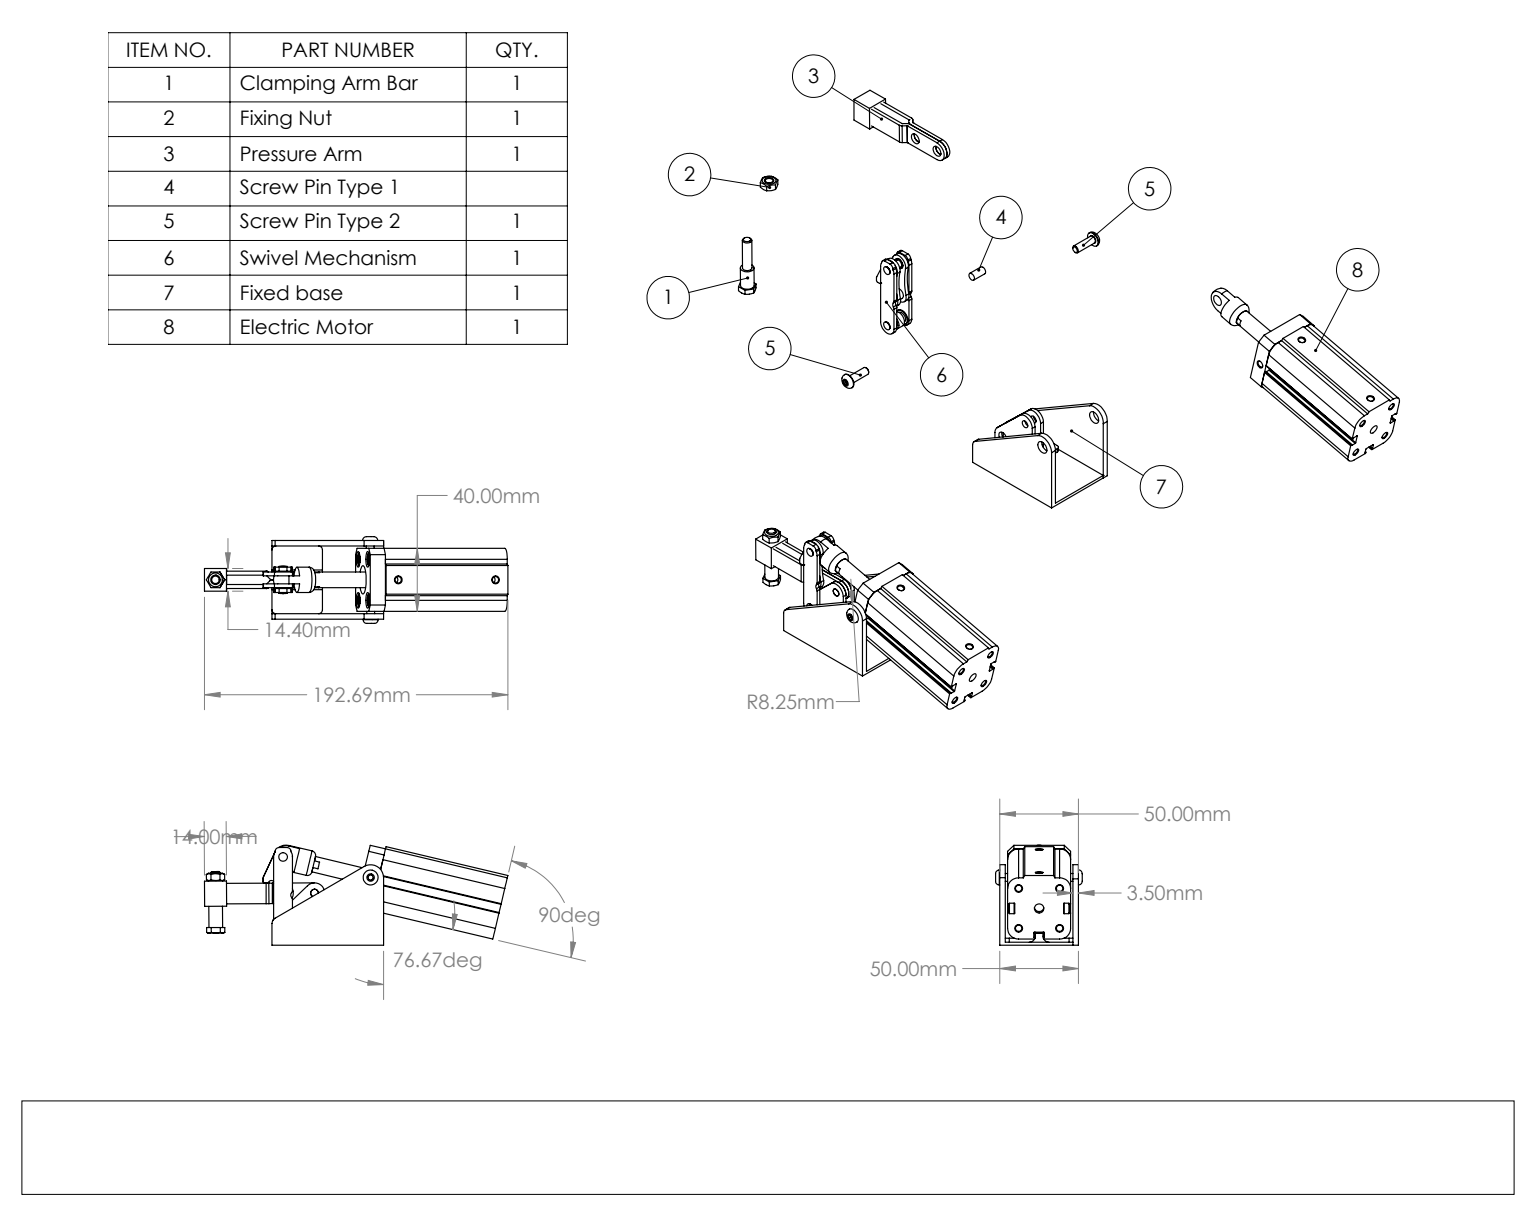
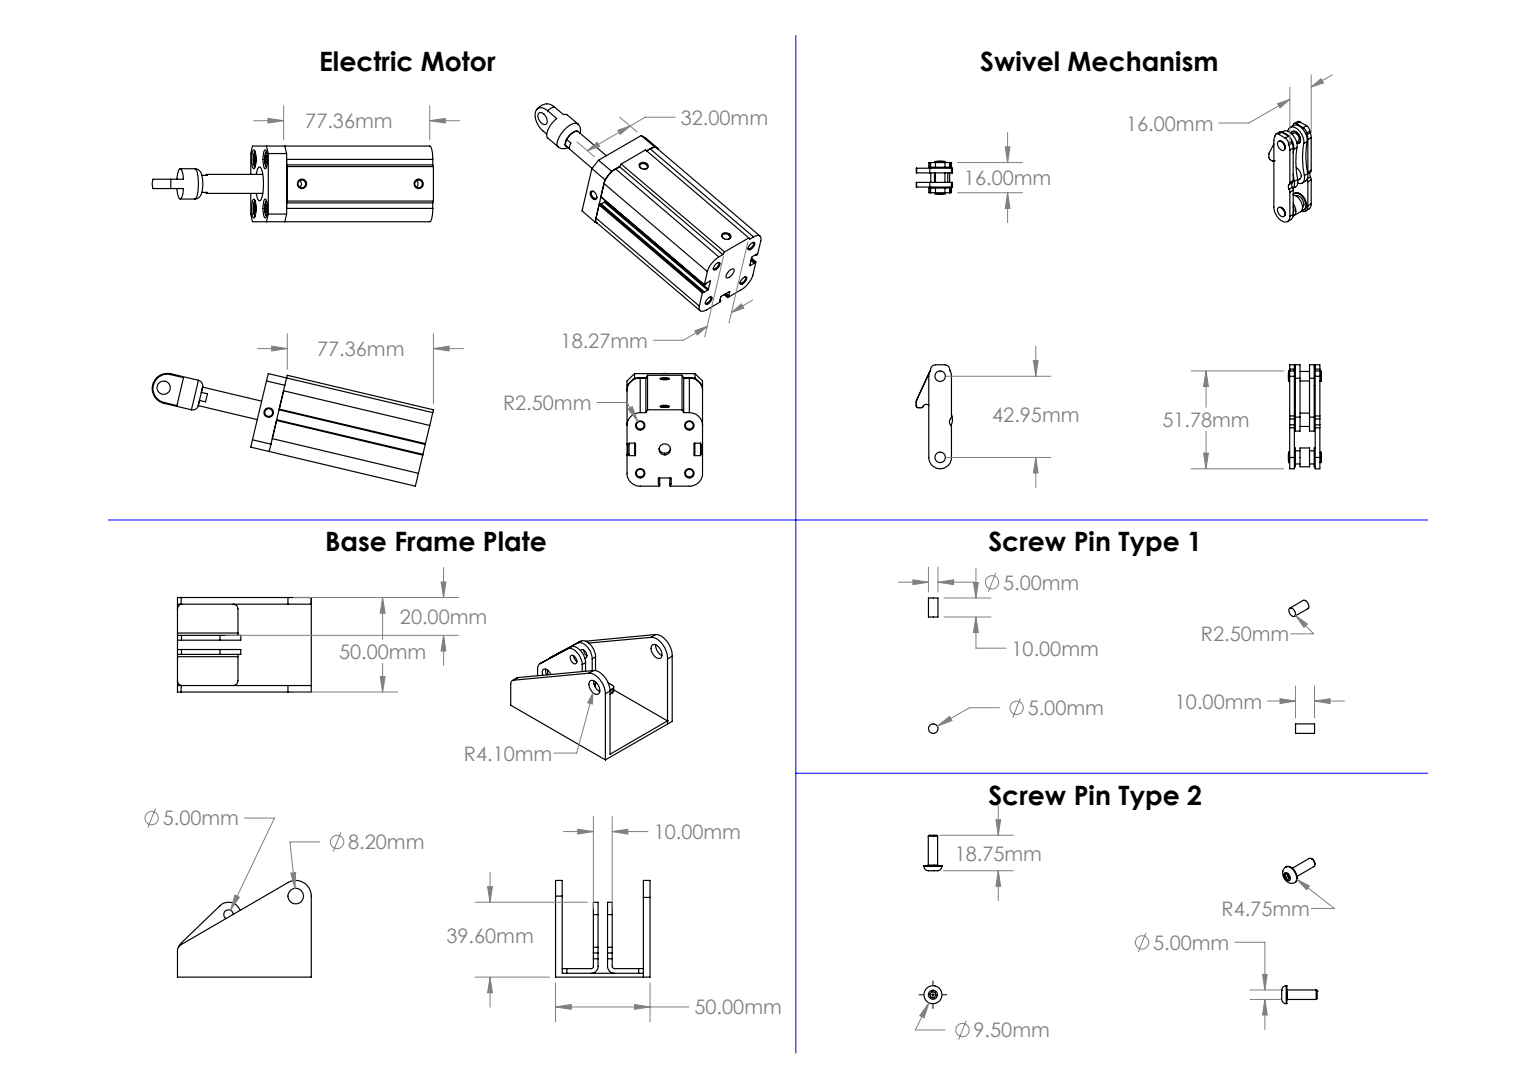
ISO-10303-21;
HEADER;
FILE_DESCRIPTION (('STEP AP203'),
    '1' );
FILE_NAME ('BR-Y-121',
    '2026-10-31T14:11:27',
    ( '' ),
    ( '' ),
    'SwSTEP 2.0',
    'SolidWorks 2024',
    '' );
FILE_SCHEMA (( 'AUTOMOTIVE_DESIGN' ));
ENDSEC;

DATA;
#1 = APPROVAL_PERSON_ORGANIZATION ( #6203, #14233, #2628 ) ;
#2 = DIRECTION ( 'NONE',  ( -0.9730401042858035643, 0.2306359803922028717, 5.958148513035547083E-17 ) ) ;
#3 = AXIS2_PLACEMENT_3D ( 'NONE', #15505, #7827, #17532 ) ;
#4 = DIRECTION ( 'NONE',  ( 1.000000000000000000, 0.000000000000000000, 0.000000000000000000 ) ) ;
#5 = CIRCLE ( 'NONE', #20894, 5.000000000000000000 ) ;
#6 = ORIENTED_EDGE ( 'NONE', *, *, #3696, .T. ) ;
#7 = PERSON ( 'NAUO-PER9', 'UNSPECIFIED', 'UNSPECIFIED', ('UNSPECIFIED'), ('UNSPECIFIED'), ('UNSPECIFIED') ) ;
#8 = CARTESIAN_POINT ( 'NONE',  ( -14.54830929633810044, -2.787889851644860251, 8.000000000004460432 ) ) ;
#9 = PERSON_AND_ORGANIZATION ( #11966, #8758 ) ;
#10 = FACE_OUTER_BOUND ( 'NONE', #10461, .T. ) ;
#11 = CARTESIAN_POINT ( 'NONE',  ( 34.15720538308221421, 9.344634530308759679, 27.44000000000022865 ) ) ;
#12 = CARTESIAN_POINT ( 'NONE',  ( 35.59419854219520118, 9.774809681453518806, 20.00000000000000000 ) ) ;
#13 = LOCAL_TIME ( 14, 11, 27.00000000000000000, #9898 ) ;
#14 = DIRECTION ( 'NONE',  ( -0.2306359803922088947, -0.9730401042858021210, 5.139921410301650007E-15 ) ) ;
#15 = CARTESIAN_POINT ( 'NONE',  ( -20.00000000000000000, -20.00000000000000000, 5.000000000004559908 ) ) ;
#16 = APPROVAL_PERSON_ORGANIZATION ( #20462, #778, #17266 ) ;
#17 = ORIENTED_EDGE ( 'NONE', *, *, #3530, .T. ) ;
#18 = CARTESIAN_POINT ( 'NONE',  ( 33.99815084691889666, 11.09517226956036673, 8.954072598562477836 ) ) ;
#19 = ADVANCED_FACE ( 'NONE', ( #17012 ), #726, .F. ) ;
#20 = AXIS2_PLACEMENT_3D ( 'NONE', #1988, #305, #1861 ) ;
#21 = ADVANCED_FACE ( 'NONE', ( #855, #17968 ), #19734, .F. ) ;
#22 = EDGE_LOOP ( 'NONE', ( #6663, #15564, #14189, #16631, #9667 ) ) ;
#23 = LINE ( 'NONE', #23425, #95 ) ;
#24 = DIRECTION ( 'NONE',  ( -0.9999862922474493931, -0.005235963827107929618, 0.000000000000000000 ) ) ;
#25 = EDGE_LOOP ( 'NONE', ( #13896, #19645, #1071, #1606 ) ) ;
#26 = VECTOR ( 'NONE', #14901, 1000.000000000000000 ) ;
#27 = FACE_OUTER_BOUND ( 'NONE', #19207, .T. ) ;
#28 = ORIENTED_EDGE ( 'NONE', *, *, #3722, .T. ) ;
#29 = CYLINDRICAL_SURFACE ( 'NONE', #10267, 4.750000000000001776 ) ;
#30 = PERSON_AND_ORGANIZATION ( #11966, #8758 ) ;
#31 = CARTESIAN_POINT ( 'NONE',  ( -62.94230935805129690, 13.36384453327990052, -5.515482965309170069E-15 ) ) ;
#32 = EDGE_CURVE ( 'NONE', #6326, #3176, #10614, .T. ) ;
#33 = EDGE_CURVE ( 'NONE', #13752, #1171, #21401, .T. ) ;
#34 = LOCAL_TIME ( 14, 11, 27.00000000000000000, #7017 ) ;
#35 =( LENGTH_UNIT ( ) NAMED_UNIT ( * ) SI_UNIT ( .MILLI., .METRE. ) );
#36 = CC_DESIGN_SECURITY_CLASSIFICATION ( #2323, ( #4225 ) ) ;
#37 = VECTOR ( 'NONE', #8550, 1000.000000000000000 ) ;
#38 = CARTESIAN_POINT ( 'NONE',  ( -18.05391955182270181, 22.49081825942809942, -4.900728725074969882E-15 ) ) ;
#39 = DIRECTION ( 'NONE',  ( -2.982858504577314686E-17, 2.441916418604790135E-15, 1.000000000000000000 ) ) ;
#40 = DIRECTION ( 'NONE',  ( 0.000000000000000000, 0.000000000000000000, 1.000000000000000000 ) ) ;
#41 = CC_DESIGN_SECURITY_CLASSIFICATION ( #8779, ( #23492 ) ) ;
#42 = DIRECTION ( 'NONE',  ( 2.269747459788994803E-13, 2.220446049250620342E-15, 1.000000000000000000 ) ) ;
#43 = CARTESIAN_POINT ( 'NONE',  ( 0.000000000000000000, 0.000000000000000000, -5.000000000000000000 ) ) ;
#44 = FACE_OUTER_BOUND ( 'NONE', #302, .T. ) ;
#45 = CYLINDRICAL_SURFACE ( 'NONE', #4982, 2.499999999999998668 ) ;
#46 = CARTESIAN_POINT ( 'NONE',  ( -14.70588235717489844, 25.77561860482770228, 6.750000000004400036 ) ) ;
#47 = CARTESIAN_POINT ( 'NONE',  ( -19.99995718853209681, 22.95166395734839782, 5.000000000000000000 ) ) ;
#48 = ORIENTED_EDGE ( 'NONE', *, *, #17410, .F. ) ;
#49 = ADVANCED_FACE ( 'NONE', ( #3230, #23291, #10261, #6805 ), #6927, .T. ) ;
#50 = APPROVAL_PERSON_ORGANIZATION ( #1727, #3134, #5184 ) ;
#51 = ORIENTED_EDGE ( 'NONE', *, *, #216, .T. ) ;
#52 = DIRECTION ( 'NONE',  ( 0.9999862922474493931, 0.005235963827110273229, 0.000000000000000000 ) ) ;
#53 = CARTESIAN_POINT ( 'NONE',  ( 37.91003399039540511, 9.225896048120093340, 26.88000000000000611 ) ) ;
#54 = VERTEX_POINT ( 'NONE', #10385 ) ;
#55 = TOROIDAL_SURFACE ( 'NONE', #1961, 3.750000000000000000, 0.5000000000000000000 ) ;
#57 = APPROVAL_ROLE ( '' ) ;
#56 = CC_DESIGN_DATE_AND_TIME_ASSIGNMENT ( #6154, #2482, ( #6812 ) ) ;
#58 = DIRECTION ( 'NONE',  ( -0.9999862922474493931, -0.005235963827110211646, -9.568357752077023983E-37 ) ) ;
#59 = ORIENTED_EDGE ( 'NONE', *, *, #12413, .F. ) ;
#60 = CC_DESIGN_DATE_AND_TIME_ASSIGNMENT ( #6062, #11785, ( #14859 ) ) ;
#61 = CARTESIAN_POINT ( 'NONE',  ( 112.5523895830310011, 2.765522746992190140, 1.033500000000031838 ) ) ;
#62 = SECURITY_CLASSIFICATION ( '', '', #11023 ) ;
#63 = DATE_AND_TIME ( #3527, #1246 ) ;
#64 = ADVANCED_FACE ( 'NONE', ( #15712 ), #3464, .F. ) ;
#65 = ADVANCED_FACE ( 'NONE', ( #10736 ), #4781, .T. ) ;
#66 = DIRECTION ( 'NONE',  ( -1.138590270679730064E-14, -2.220446049251245514E-15, -1.000000000000000000 ) ) ;
#67 = EDGE_CURVE ( 'NONE', #14097, #1408, #5016, .T. ) ;
#68 = CC_DESIGN_APPROVAL ( #5463, ( #7661 ) ) ;
#69 = FACE_OUTER_BOUND ( 'NONE', #8738, .T. ) ;
#70 = VECTOR ( 'NONE', #6316, 1000.000000000000114 ) ;
#71 = ORIENTED_EDGE ( 'NONE', *, *, #21028, .T. ) ;
#72 = DIRECTION ( 'NONE',  ( -0.9999862922474493931, -0.005235963827110373843, 0.000000000000000000 ) ) ;
#73 = CIRCLE ( 'NONE', #5027, 49.22658835543908395 ) ;
#74 = AXIS2_PLACEMENT_3D ( 'NONE', #22405, #17064, #15522 ) ;
#75 = AXIS2_PLACEMENT_3D ( 'NONE', #11008, #20130, #11135 ) ;
#76 = ORIENTED_EDGE ( 'NONE', *, *, #8643, .T. ) ;
#77 = CC_DESIGN_SECURITY_CLASSIFICATION ( #22065, ( #23506 ) ) ;
#78 = DIRECTION ( 'NONE',  ( -0.9997651245102161521, -0.02167246670483388357, 0.000000000000000000 ) ) ;
#79 = CARTESIAN_POINT ( 'NONE',  ( 41.24356139695900225, 11.92996613406550033, 15.90000000000000036 ) ) ;
#80 = DIRECTION ( 'NONE',  ( -1.159535895544890222E-14, -2.167612681253619929E-15, -1.000000000000000000 ) ) ;
#81 = ORIENTED_EDGE ( 'NONE', *, *, #7510, .T. ) ;
#82 = AXIS2_PLACEMENT_3D ( 'NONE', #367, #4066, #9672 ) ;
#83 = EDGE_CURVE ( 'NONE', #7095, #13655, #23162, .T. ) ;
#84 = CARTESIAN_POINT ( 'NONE',  ( 5.000000000000000000, -29.85000000000000142, -12.00000000000000000 ) ) ;
#85 = AXIS2_PLACEMENT_3D ( 'NONE', #8202, #22670, #2860 ) ;
#86 = EDGE_LOOP ( 'NONE', ( #14496, #4097, #19761, #7467 ) ) ;
#87 = DATE_TIME_ROLE ( 'creation_date' ) ;
#88 = CC_DESIGN_APPROVAL ( #11152, ( #18095 ) ) ;
#89 = ORIENTED_EDGE ( 'NONE', *, *, #15771, .F. ) ;
#90 = VERTEX_POINT ( 'NONE', #12158 ) ;
#91 = DIRECTION ( 'NONE',  ( 6.123230174520380038E-17, 4.962644601432250805E-15, 1.000000000000000000 ) ) ;
#92 = CALENDAR_DATE ( 2026, 31, 10 ) ;
#93 = VECTOR ( 'NONE', #17337, 1000.000000000000000 ) ;
#94 = EDGE_CURVE ( 'NONE', #17862, #6798, #19506, .T. ) ;
#95 = VECTOR ( 'NONE', #9188, 1000.000000000000227 ) ;
#96 = EDGE_CURVE ( 'NONE', #14120, #3226, #13723, .T. ) ;
#97 = CARTESIAN_POINT ( 'NONE',  ( -20.00000000397270128, 22.95208919256889857, -4.999999999995559996 ) ) ;
#98 = SECURITY_CLASSIFICATION_LEVEL ( 'unclassified' ) ;
#99 = CARTESIAN_POINT ( 'NONE',  ( 63.21106856953390007, 5.468723628172329931, -4.500000000000000000 ) ) ;
#100 = DIRECTION ( 'NONE',  ( 0.1153179901961009640, 0.4865200521429018377, 0.8660254037844385966 ) ) ;
#101 = CIRCLE ( 'NONE', #2773, 2.066999999999999282 ) ;
#102 = PERSON_AND_ORGANIZATION_ROLE ( 'creator' ) ;
#103 = LOCAL_TIME ( 14, 11, 27.00000000000000000, #5648 ) ;
#104 = VERTEX_POINT ( 'NONE', #3345 ) ;
#105 = CIRCLE ( 'NONE', #10016, 1.000000000000000000 ) ;
#106 = DIRECTION ( 'NONE',  ( -0.9730401042858035643, 0.2306359803922028717, 5.958148513035547083E-17 ) ) ;
#107 = ORIENTED_EDGE ( 'NONE', *, *, #9525, .T. ) ;
#108 = EDGE_CURVE ( 'NONE', #467, #12098, #6515, .T. ) ;
#109 = CARTESIAN_POINT ( 'NONE',  ( -64.07944010525029910, -25.33596492959100388, 4.999999999999991118 ) ) ;
#110 = AXIS2_PLACEMENT_3D ( 'NONE', #13114, #22230, #618 ) ;
#111 = CARTESIAN_POINT ( 'NONE',  ( -14.00000000144730095, -4.350228928435719844, 8.000000000004460432 ) ) ;
#112 = ORIENTED_EDGE ( 'NONE', *, *, #10125, .F. ) ;
#113 = ORIENTED_EDGE ( 'NONE', *, *, #18987, .F. ) ;
#114 = CARTESIAN_POINT ( 'NONE',  ( -17.00058718854806017, -0.04792152746387602635, 2.500000000000000000 ) ) ;
#115 = VERTEX_POINT ( 'NONE', #8937 ) ;
#116 = DATE_AND_TIME ( #9155, #9125 ) ;
#117 = ADVANCED_FACE ( 'NONE', ( #23398 ), #23180, .F. ) ;
#118 = EDGE_CURVE ( 'NONE', #1889, #6893, #1553, .T. ) ;
#119 = ORIENTED_EDGE ( 'NONE', *, *, #12198, .T. ) ;
#120 = ORIENTED_EDGE ( 'NONE', *, *, #19486, .F. ) ;
#121 = LINE ( 'NONE', #10734, #5080 ) ;
#122 = CIRCLE ( 'NONE', #15304, 1.250000000000000222 ) ;
#123 = CARTESIAN_POINT ( 'NONE',  ( 50.76434296088209663, 17.41090750189739822, 1.033500000000035390 ) ) ;
#124 = PERSON_AND_ORGANIZATION ( #11966, #8758 ) ;
#125 = EDGE_CURVE ( 'NONE', #15552, #9993, #3113, .T. ) ;
#126 = DIRECTION ( 'NONE',  ( 3.837966487416234409E-32, -1.216195237911450118E-15, -1.000000000000000000 ) ) ;
#127 = LOCAL_TIME ( 14, 11, 27.00000000000000000, #22000 ) ;
#128 = AXIS2_PLACEMENT_3D ( 'NONE', #20499, #7802, #13149 ) ;
#129 = ADVANCED_FACE ( 'NONE', ( #12049 ), #13926, .T. ) ;
#130 = CARTESIAN_POINT ( 'NONE',  ( -22.49917142882856069, 22.89791325974001879, 4.999999999999900524 ) ) ;
#131 = VERTEX_POINT ( 'NONE', #18186 ) ;
#132 = LINE ( 'NONE', #14633, #21183 ) ;
#133 = DATE_AND_TIME ( #14747, #21292 ) ;
#134 = VERTEX_POINT ( 'NONE', #20076 ) ;
#135 = DIRECTION ( 'NONE',  ( -1.000000000000000000, 0.000000000000000000, 0.000000000000000000 ) ) ;
#136 = FACE_OUTER_BOUND ( 'NONE', #13808, .T. ) ;
#137 = CARTESIAN_POINT ( 'NONE',  ( 31.37708959083939675, -0.2124270449897310287, 13.00000000000019895 ) ) ;
#138 = CIRCLE ( 'NONE', #3191, 2.500000000000000000 ) ;
#139 = CARTESIAN_POINT ( 'NONE',  ( 34.40556712239440174, 8.514986143070938596, -28.47000000000049980 ) ) ;
#140 =( BOUNDED_CURVE ( )  B_SPLINE_CURVE ( 2, ( #4073, #2529, #968 ),
 .UNSPECIFIED., .F., .F. ) 
 B_SPLINE_CURVE_WITH_KNOTS ( ( 3, 3 ),
 ( 0.000000000000000000, 0.2336872276155859962 ),
 .UNSPECIFIED. ) 
 CURVE ( )  GEOMETRIC_REPRESENTATION_ITEM ( )  RATIONAL_B_SPLINE_CURVE ( ( 1.000000000000000000, 1.154700538379259900, 1.000000000000000000 ) ) 
 REPRESENTATION_ITEM ( '' )  );
#141 = CYLINDRICAL_SURFACE ( 'NONE', #14862, 5.000000000000000888 ) ;
#142 = VERTEX_POINT ( 'NONE', #16617 ) ;
#143 = AXIS2_PLACEMENT_3D ( 'NONE', #12273, #14149, #12491 ) ;
#144 = CARTESIAN_POINT ( 'NONE',  ( 34.27408172216480153, 8.178586146432554216, 8.806355889830941308 ) ) ;
#145 = UNCERTAINTY_MEASURE_WITH_UNIT (LENGTH_MEASURE( 1.000000000000000082E-05 ), #895, 'distance_accuracy_value', 'NONE');
#146 = CC_DESIGN_DATE_AND_TIME_ASSIGNMENT ( #5252, #8837, ( #6840 ) ) ;
#147 = ORIENTED_EDGE ( 'NONE', *, *, #4410, .F. ) ;
#148 = CARTESIAN_POINT ( 'NONE',  ( 118.5310588935630136, -6.697506338400800452, -20.00000000000000000 ) ) ;
#149 = CARTESIAN_POINT ( 'NONE',  ( -27.00000000000000000, -27.34999999999999787, 6.250000000000000000 ) ) ;
#150 = ORIENTED_EDGE ( 'NONE', *, *, #9051, .F. ) ;
#151 = PLANE ( 'NONE',  #7708 ) ;
#152 = ORIENTED_EDGE ( 'NONE', *, *, #1613, .T. ) ;
#153 = CARTESIAN_POINT ( 'NONE',  ( 35.09747506357100377, 11.43410645592840069, -27.69000000000049866 ) ) ;
#154 = PERSON_AND_ORGANIZATION ( #11966, #8758 ) ;
#155 = PLANE ( 'NONE',  #7113 ) ;
#156 = APPLICATION_CONTEXT ( 'configuration controlled 3d designs of mechanical parts and assemblies' ) ;
#157 = PLANE ( 'NONE',  #11148 ) ;
#158 = EDGE_CURVE ( 'NONE', #20720, #6814, #11078, .T. ) ;
#159 = CARTESIAN_POINT ( 'NONE',  ( -14.00000000000000000, -19.99999999944489915, 5.500000000004489742 ) ) ;
#160 = CARTESIAN_POINT ( 'NONE',  ( -20.00000000397459843, 22.95208919257349933, -7.999999999995569766 ) ) ;
#161 = DIRECTION ( 'NONE',  ( -2.982858504489129897E-17, 2.441916418604790135E-15, 1.000000000000000000 ) ) ;
#162 = CARTESIAN_POINT ( 'NONE',  ( -62.91331795724000386, 7.826945432762889787, -2.729132938682638176 ) ) ;
#163 = DESIGN_CONTEXT ( 'detailed design', #14471, 'design' ) ;
#164 = CARTESIAN_POINT ( 'NONE',  ( 0.000000000000000000, -17.30000000000000071, -2.500000000000000000 ) ) ;
#165 = CARTESIAN_POINT ( 'NONE',  ( 43.84419854219520829, -31.09999999999999787, 21.49999999999999289 ) ) ;
#166 = DIRECTION ( 'NONE',  ( -0.005235963827117092427, 0.9999862922474493931, 2.636227439667000721E-16 ) ) ;
#167 = ORIENTED_EDGE ( 'NONE', *, *, #12338, .T. ) ;
#168 = EDGE_LOOP ( 'NONE', ( #10288, #18561, #2673, #1154, #10285 ) ) ;
#169 = DIRECTION ( 'NONE',  ( -9.594916218540590128E-33, 2.583840697242805182E-16, -1.000000000000000000 ) ) ;
#170 = DIRECTION ( 'NONE',  ( 0.2306359803922080343, 0.9730401042858022320, 7.611545645951921999E-14 ) ) ;
#171 = VERTEX_POINT ( 'NONE', #5590 ) ;
#172 = DIRECTION ( 'NONE',  ( -2.977235988022386522E-185, 9.605990953944227443E-124, 1.000000000000000000 ) ) ;
#173 = ORIENTED_EDGE ( 'NONE', *, *, #19680, .T. ) ;
#174 = DIRECTION ( 'NONE',  ( -0.04564792618500997101, -0.9989575901083128651, 2.775557561562890562E-15 ) ) ;
#175 = APPROVAL_DATE_TIME ( #63, #347 ) ;
#176 = CARTESIAN_POINT ( 'NONE',  ( 36.18988576660174061, 7.790900190088850152, -8.819913685435235351 ) ) ;
#177 = PRODUCT_DEFINITION_SHAPE ( 'NONE', 'NONE',  #10711 ) ;
#178 = PERSON_AND_ORGANIZATION ( #18420, #6505 ) ;
#179 = CYLINDRICAL_SURFACE ( 'NONE', #16897, 2.066999999999999726 ) ;
#180 = ORIENTED_EDGE ( 'NONE', *, *, #10830, .F. ) ;
#181 = ADVANCED_FACE ( 'NONE', ( #7395 ), #2255, .T. ) ;
#182 = AXIS2_PLACEMENT_3D ( 'NONE', #3666, #10943, #21940 ) ;
#183 = CARTESIAN_POINT ( 'NONE',  ( 114.1489752661110089, -25.18526831983100323, 3.399999999999999911 ) ) ;
#184 = VERTEX_POINT ( 'NONE', #1903 ) ;
#185 = CARTESIAN_POINT ( 'NONE',  ( 118.6002496876800052, -6.405594307115129560, 18.89999999999999858 ) ) ;
#186 = CC_DESIGN_PERSON_AND_ORGANIZATION_ASSIGNMENT ( #15049, #22282, ( #17552 ) ) ;
#187 = VERTEX_POINT ( 'NONE', #3798 ) ;
#188 = LINE ( 'NONE', #7456, #8973 ) ;
#189 = CYLINDRICAL_SURFACE ( 'NONE', #19053, 2.750000000000000000 ) ;
#190 = DIRECTION ( 'NONE',  ( -0.2306359803922032603, -0.9730401042858035643, 4.741332172907965995E-18 ) ) ;
#191 = ORIENTED_EDGE ( 'NONE', *, *, #19640, .F. ) ;
#192 = EDGE_CURVE ( 'NONE', #3524, #19301, #10707, .T. ) ;
#193 = ADVANCED_FACE ( 'NONE', ( #7501 ), #14386, .T. ) ;
#194 = PERSON_AND_ORGANIZATION ( #4548, #19443 ) ;
#195 = CARTESIAN_POINT ( 'NONE',  ( -27.00000000000000000, -27.34999999999999787, -2.500000000000000000 ) ) ;
#196 = ORIENTED_EDGE ( 'NONE', *, *, #12338, .F. ) ;
#197 = PERSON_AND_ORGANIZATION_ROLE ( 'design_owner' ) ;
#198 = ORIENTED_EDGE ( 'NONE', *, *, #5195, .T. ) ;
#199 = VERTEX_POINT ( 'NONE', #2140 ) ;
#200 = DIRECTION ( 'NONE',  ( -6.123237832262829536E-17, -1.734723475976808278E-15, 1.000000000000000000 ) ) ;
#201 = PERSON_AND_ORGANIZATION ( #11966, #8758 ) ;
#202 = VECTOR ( 'NONE', #1831, 1000.000000000000114 ) ;
#203 = CARTESIAN_POINT ( 'NONE',  ( 34.89491389100820129, 23.30074776265919922, 13.00000000000000000 ) ) ;
#204 = PERSON_AND_ORGANIZATION ( #11064, #10995 ) ;
#205 = DIRECTION ( 'NONE',  ( 0.02168293104353429326, -0.9997648976141146893, 2.442038521257509372E-15 ) ) ;
#206 = ADVANCED_FACE ( 'NONE', ( #12841 ), #9161, .T. ) ;
#207 = DIRECTION ( 'NONE',  ( -0.9730401042858022320, 0.2306359803922080343, 5.959266323858941219E-17 ) ) ;
#208 = CC_DESIGN_PERSON_AND_ORGANIZATION_ASSIGNMENT ( #13871, #21104, ( #17062 ) ) ;
#209 = DATE_AND_TIME ( #15069, #18208 ) ;
#210 =( GEOMETRIC_REPRESENTATION_CONTEXT ( 3 ) GLOBAL_UNCERTAINTY_ASSIGNED_CONTEXT ( ( #9838 ) ) GLOBAL_UNIT_ASSIGNED_CONTEXT ( ( #2432, #18585, #11238 ) ) REPRESENTATION_CONTEXT ( 'NONE', 'WORKASPACE' ) );
#211 = APPROVAL ( #9394, 'UNSPECIFIED' ) ;
#212 = ORIENTED_EDGE ( 'NONE', *, *, #11041, .T. ) ;
#213 = CARTESIAN_POINT ( 'NONE',  ( -14.70588235717489844, 25.77561860482770228, 5.500000000004400036 ) ) ;
#214 = ORIENTED_EDGE ( 'NONE', *, *, #2972, .F. ) ;
#215 = EDGE_CURVE ( 'NONE', #11840, #10096, #7770, .T. ) ;
#216 = EDGE_CURVE ( 'NONE', #1911, #563, #20207, .T. ) ;
#217 = AXIS2_PLACEMENT_3D ( 'NONE', #15090, #20672, #22793 ) ;
#218 = CARTESIAN_POINT ( 'NONE',  ( 2.500000000000026645, -7.535786464196452844E-15, 2.500000000000000000 ) ) ;
#219 = CC_DESIGN_PERSON_AND_ORGANIZATION_ASSIGNMENT ( #2839, #2604, ( #16680 ) ) ;
#220 = CARTESIAN_POINT ( 'NONE',  ( 29.36184298829670070, -3.294841866349740300, 15.00000000000000000 ) ) ;
#221 = DIRECTION ( 'NONE',  ( 0.9999862922474493931, 0.005235963827101436548, -1.187304881134279227E-16 ) ) ;
#222 = ORIENTED_EDGE ( 'NONE', *, *, #1641, .T. ) ;
#223 = EDGE_LOOP ( 'NONE', ( #4178, #13372, #15344, #5605 ) ) ;
#224 = DIRECTION ( 'NONE',  ( 0.2306359803922031215, 0.9730401042858033422, -1.407521210652540462E-17 ) ) ;
#225 = ORIENTED_EDGE ( 'NONE', *, *, #9354, .F. ) ;
#226 = APPROVAL_ROLE ( '' ) ;
#227 = VERTEX_POINT ( 'NONE', #5838 ) ;
#228 = EDGE_LOOP ( 'NONE', ( #11075, #14429 ) ) ;
#229 = CYLINDRICAL_SURFACE ( 'NONE', #3934, 2.500000000000000000 ) ;
#230 = DIRECTION ( 'NONE',  ( 1.187319687680494078E-16, 2.805478249478345354E-20, 1.000000000000000000 ) ) ;
#231 = COORDINATED_UNIVERSAL_TIME_OFFSET ( 0, 0, .AHEAD. ) ;
#232 = CARTESIAN_POINT ( 'NONE',  ( 37.40573311221180575, -6.139030851290243618, 13.00000000000000000 ) ) ;
#233 = AXIS2_PLACEMENT_3D ( 'NONE', #18438, #5592, #126 ) ;
#234 = CARTESIAN_POINT ( 'NONE',  ( 30.76933207471820708, -4.221800468112564708, -14.00000000000040146 ) ) ;
#235 = AXIS2_PLACEMENT_3D ( 'NONE', #21631, #7407, #21868 ) ;
#236 = EDGE_CURVE ( 'NONE', #10293, #10039, #18795, .T. ) ;
#237 =( LENGTH_UNIT ( ) NAMED_UNIT ( * ) SI_UNIT ( .MILLI., .METRE. ) );
#238 = VERTEX_POINT ( 'NONE', #344 ) ;
#239 = PLANE ( 'NONE',  #21167 ) ;
#240 = PERSON_AND_ORGANIZATION ( #11966, #8758 ) ;
#241 = EDGE_CURVE ( 'NONE', #7018, #17568, #14626, .T. ) ;
#242 = ORIENTED_EDGE ( 'NONE', *, *, #2441, .T. ) ;
#243 = CIRCLE ( 'NONE', #9002, 2.499999999999999556 ) ;
#244 = FACE_OUTER_BOUND ( 'NONE', #22549, .T. ) ;
#245 = CARTESIAN_POINT ( 'NONE',  ( -19.49999999982379961, -0.1021026942259709996, 9.160072195675308484E-14 ) ) ;
#246 = ADVANCED_FACE ( 'NONE', ( #18435 ), #4045, .T. ) ;
#247 = CARTESIAN_POINT ( 'NONE',  ( 34.40839383886530101, 23.41606575285529956, 13.00000000000000000 ) ) ;
#248 = DIRECTION ( 'NONE',  ( -6.662111519016958720E-09, 1.000000000000000000, -2.523234146875356491E-15 ) ) ;
#249 = EDGE_CURVE ( 'NONE', #9426, #18548, #22088, .T. ) ;
#250 = VECTOR ( 'NONE', #1916, 1000.000000000000000 ) ;
#251 = FACE_OUTER_BOUND ( 'NONE', #19236, .T. ) ;
#252 = VERTEX_POINT ( 'NONE', #19862 ) ;
#253 = CYLINDRICAL_SURFACE ( 'NONE', #3131, 2.650000000000001688 ) ;
#254 = ORIENTED_EDGE ( 'NONE', *, *, #5018, .F. ) ;
#255 = VERTEX_POINT ( 'NONE', #3589 ) ;
#256 = CARTESIAN_POINT ( 'NONE',  ( 117.0319250210129951, -13.02226701625849969, -15.90000000000000036 ) ) ;
#257 = DIRECTION ( 'NONE',  ( -1.159535895544890222E-14, -2.167612681253619929E-15, -1.000000000000000000 ) ) ;
#258 = VECTOR ( 'NONE', #13231, 1000.000000000000000 ) ;
#259 = ORIENTED_EDGE ( 'NONE', *, *, #16871, .F. ) ;
#260 = CARTESIAN_POINT ( 'NONE',  ( -19.99999998565371229, 20.20208919256890212, -8.499999999995543121 ) ) ;
#261 = ORIENTED_EDGE ( 'NONE', *, *, #549, .T. ) ;
#262 = DIRECTION ( 'NONE',  ( -0.9997651245102238127, -0.02167246670447303680, 0.000000000000000000 ) ) ;
#263 = AXIS2_PLACEMENT_3D ( 'NONE', #10601, #1540, #1662 ) ;
#264 = DATE_TIME_ROLE ( 'classification_date' ) ;
#265 = DIRECTION ( 'NONE',  ( 0.000000000000000000, -1.000000000000000000, 9.355573283744330345E-16 ) ) ;
#266 = VECTOR ( 'NONE', #19546, 1000.000000000000000 ) ;
#267 = AXIS2_PLACEMENT_3D ( 'NONE', #2294, #14886, #3727 ) ;
#268 = CIRCLE ( 'NONE', #7866, 3.499999999999999556 ) ;
#269 = SHAPE_REPRESENTATION_RELATIONSHIP ( 'NONE' , 'NONE' ,  #488, #12210 ) ;
#270 = CARTESIAN_POINT ( 'NONE',  ( 35.06754128096959988, 7.552872603316886035, 19.78350000000001074 ) ) ;
#271 = FACE_OUTER_BOUND ( 'NONE', #1548, .T. ) ;
#272 = DATE_TIME_ROLE ( 'creation_date' ) ;
#273 = DIRECTION ( 'NONE',  ( 2.269747459788990007E-13, 2.220446049250330436E-15, 1.000000000000000000 ) ) ;
#274 = AXIS2_PLACEMENT_3D ( 'NONE', #4607, #15649, #6504 ) ;
#275 = DIRECTION ( 'NONE',  ( -1.000000000000000000, 0.000000000000000000, 0.000000000000000000 ) ) ;
#276 = DIRECTION ( 'NONE',  ( 6.123230174520380038E-17, 4.962644601432250805E-15, 1.000000000000000000 ) ) ;
#277 = CARTESIAN_POINT ( 'NONE',  ( 2.500000000000000000, -30.47499999999999787, -21.50000000000000000 ) ) ;
#278 = CARTESIAN_POINT ( 'NONE',  ( 28.41185834866789861, -1.882976958576189963, -13.00000000000039968 ) ) ;
#279 = CARTESIAN_POINT ( 'NONE',  ( -22.52506283708569867, 28.95208917575130414, 8.000000000004481748 ) ) ;
#280 = ORIENTED_EDGE ( 'NONE', *, *, #13563, .F. ) ;
#281 = AXIS2_PLACEMENT_3D ( 'NONE', #8014, #22242, #9805 ) ;
#282 = ORIENTED_EDGE ( 'NONE', *, *, #4334, .T. ) ;
#283 = DIRECTION ( 'NONE',  ( 0.000000000000000000, -2.755911201911430512E-15, -1.000000000000000000 ) ) ;
#284 = AXIS2_PLACEMENT_3D ( 'NONE', #13353, #20118, #2539 ) ;
#285 = CARTESIAN_POINT ( 'NONE',  ( -1.077004981755310231, 16.07039212396449912, -4.500000000000000000 ) ) ;
#286 = ORIENTED_EDGE ( 'NONE', *, *, #15419, .F. ) ;
#287 = PERSON ( 'NAUO-PER19', 'UNSPECIFIED', 'UNSPECIFIED', ('UNSPECIFIED'), ('UNSPECIFIED'), ('UNSPECIFIED') ) ;
#288 = CARTESIAN_POINT ( 'NONE',  ( 2.500000000000000000, -28.60000000000000142, -19.00000000000000000 ) ) ;
#289 = EDGE_CURVE ( 'NONE', #8641, #12606, #10851, .T. ) ;
#290 = VERTEX_POINT ( 'NONE', #14509 ) ;
#291 = CARTESIAN_POINT ( 'NONE',  ( 36.76586756491558816, 21.07724224331888863, 12.00000000000000000 ) ) ;
#292 = DATE_AND_TIME ( #14793, #2017 ) ;
#293 = LINE ( 'NONE', #15380, #15436 ) ;
#294 = PERSON_AND_ORGANIZATION_ROLE ( 'classification_officer' ) ;
#295 = VECTOR ( 'NONE', #19541, 1000.000000000000000 ) ;
#296 = DIRECTION ( 'NONE',  ( 1.751019220569994795E-16, 2.300154215587015208E-15, 1.000000000000000000 ) ) ;
#297 = ORIENTED_EDGE ( 'NONE', *, *, #15434, .T. ) ;
#298 = CIRCLE ( 'NONE', #13970, 5.000000000000004441 ) ;
#299 = CARTESIAN_POINT ( 'NONE',  ( 44.19498725252769589, 23.44315552359092791, 13.00000000000000000 ) ) ;
#300 = VERTEX_POINT ( 'NONE', #21746 ) ;
#301 = CARTESIAN_POINT ( 'NONE',  ( 118.4388045014059969, -7.086722380115170417, -18.89999999999999858 ) ) ;
#302 = EDGE_LOOP ( 'NONE', ( #2041, #9223, #15039, #5086 ) ) ;
#303 = DIRECTION ( 'NONE',  ( 0.8511275218278948618, 0.5249589903860170104, -5.212440122911309516E-17 ) ) ;
#304 = CARTESIAN_POINT ( 'NONE',  ( 58.49563186522070168, 17.70675969991879839, -15.25462000000050011 ) ) ;
#305 = DIRECTION ( 'NONE',  ( -1.138590270679734009E-14, -2.220446049251240387E-15, -1.000000000000000000 ) ) ;
#306 = VERTEX_POINT ( 'NONE', #5482 ) ;
#307 = CALENDAR_DATE ( 2026, 31, 10 ) ;
#308 = DIRECTION ( 'NONE',  ( -1.000000000000000000, 0.000000000000000000, 0.000000000000000000 ) ) ;
#309 = ORIENTED_EDGE ( 'NONE', *, *, #22135, .T. ) ;
#310 = EDGE_CURVE ( 'NONE', #20720, #14320, #1201, .T. ) ;
#311 = DATE_AND_TIME ( #22287, #8011 ) ;
#312 = DIRECTION ( 'NONE',  ( 7.664170260637049561E-16, 3.491853980616970288E-15, -1.000000000000000000 ) ) ;
#313 = EDGE_CURVE ( 'NONE', #8111, #8468, #10967, .T. ) ;
#314 = ORIENTED_EDGE ( 'NONE', *, *, #22865, .F. ) ;
#315 = ORIENTED_EDGE ( 'NONE', *, *, #19389, .F. ) ;
#316 = CLOSED_SHELL ( 'NONE', ( #181, #9383, #7532, #3257, #22716, #15891 ) ) ;
#317 = FACE_BOUND ( 'NONE', #5832, .T. ) ;
#318 = CIRCLE ( 'NONE', #13611, 3.499999999999999556 ) ;
#319 = DATE_AND_TIME ( #2001, #5406 ) ;
#320 = CARTESIAN_POINT ( 'NONE',  ( -20.00000000397420052, 22.95208919256889857, -6.499999999995379696 ) ) ;
#321 = CARTESIAN_POINT ( 'NONE',  ( -32.42710143188249816, 10.33427914179039853, 5.000000000000000000 ) ) ;
#322 = CIRCLE ( 'NONE', #3373, 2.369999999999999218 ) ;
#323 = EDGE_CURVE ( 'NONE', #7718, #22958, #10828, .T. ) ;
#324 = ADVANCED_FACE ( 'NONE', ( #917 ), #12711, .F. ) ;
#325 = DIRECTION ( 'NONE',  ( -0.2306359803922010121, -0.9730401042858040084, 0.000000000000000000 ) ) ;
#326 = APPROVAL_DATE_TIME ( #16602, #15773 ) ;
#327 = ORIENTED_EDGE ( 'NONE', *, *, #22096, .F. ) ;
#328 = APPLICATION_CONTEXT ( 'configuration controlled 3d designs of mechanical parts and assemblies' ) ;
#329 = CARTESIAN_POINT ( 'NONE',  ( 37.27955344062029752, 9.375336445360510140, -29.25000000000050093 ) ) ;
#330 = ORIENTED_EDGE ( 'NONE', *, *, #2152, .T. ) ;
#331 = CARTESIAN_POINT ( 'NONE',  ( 35.24824457160689661, 8.315249525024576371, -27.55602540378494325 ) ) ;
#332 = PLANE ( 'NONE',  #10040 ) ;
#333 = CYLINDRICAL_SURFACE ( 'NONE', #19089, 2.066999999999997062 ) ;
#334 = ORIENTED_EDGE ( 'NONE', *, *, #11761, .F. ) ;
#335 = CC_DESIGN_SECURITY_CLASSIFICATION ( #10620, ( #23487 ) ) ;
#336 = ORIENTED_EDGE ( 'NONE', *, *, #4633, .T. ) ;
#337 = DIRECTION ( 'NONE',  ( -2.269747459788994803E-13, -2.220446049250715400E-15, -1.000000000000000000 ) ) ;
#338 = ORIENTED_EDGE ( 'NONE', *, *, #96, .T. ) ;
#339 = COORDINATED_UNIVERSAL_TIME_OFFSET ( 0, 0, .AHEAD. ) ;
#340 = ADVANCED_FACE ( 'NONE', ( #13754 ), #20997, .F. ) ;
#341 = VERTEX_POINT ( 'NONE', #22760 ) ;
#342 = ORIENTED_EDGE ( 'NONE', *, *, #13446, .T. ) ;
#343 = DIRECTION ( 'NONE',  ( -0.9730401042858036753, 0.2306359803922031493, 5.432877459303543355E-17 ) ) ;
#344 = CARTESIAN_POINT ( 'NONE',  ( -19.80660126203780180, 15.09635365252939998, -2.500000000000000000 ) ) ;
#345 = DATE_TIME_ROLE ( 'creation_date' ) ;
#346 = CARTESIAN_POINT ( 'NONE',  ( 38.13838090529419844, 22.53196116135185179, 13.00000000000000000 ) ) ;
#347 = APPROVAL ( #14331, 'UNSPECIFIED' ) ;
#348 = CC_DESIGN_PERSON_AND_ORGANIZATION_ASSIGNMENT ( #21617, #19968, ( #15633 ) ) ;
#349 = CYLINDRICAL_SURFACE ( 'NONE', #19361, 3.499999999999998668 ) ;
#350 = EDGE_CURVE ( 'NONE', #15518, #357, #2469, .T. ) ;
#351 = EDGE_CURVE ( 'NONE', #2950, #23008, #5497, .T. ) ;
#352 = EDGE_CURVE ( 'NONE', #17009, #12811, #11602, .T. ) ;
#353 = SHAPE_REPRESENTATION_RELATIONSHIP ( 'NONE' , 'NONE' ,  #4456, #9686 ) ;
#354 = AXIS2_PLACEMENT_3D ( 'NONE', #13719, #17407, #13844 ) ;
#355 =( GEOMETRIC_REPRESENTATION_CONTEXT ( 3 ) GLOBAL_UNCERTAINTY_ASSIGNED_CONTEXT ( ( #11100 ) ) GLOBAL_UNIT_ASSIGNED_CONTEXT ( ( #15211, #22451, #20788 ) ) REPRESENTATION_CONTEXT ( 'NONE', 'WORKASPACE' ) );
#356 = VECTOR ( 'NONE', #17095, 1000.000000000000000 ) ;
#357 = VERTEX_POINT ( 'NONE', #13631 ) ;
#358 = CARTESIAN_POINT ( 'NONE',  ( 60.98218416654081864, 14.99311160239461316, -13.00000000000000000 ) ) ;
#359 = CALENDAR_DATE ( 2026, 31, 10 ) ;
#360 = EDGE_LOOP ( 'NONE', ( #4752, #20568 ) ) ;
#361 = LINE ( 'NONE', #2404, #15555 ) ;
#362 = CARTESIAN_POINT ( 'NONE',  ( 63.21106856953390007, 5.468723628172310391, 4.500000000000000000 ) ) ;
#363 = CIRCLE ( 'NONE', #383, 2.700000000000000178 ) ;
#364 = DIRECTION ( 'NONE',  ( 0.000000000000000000, 0.000000000000000000, 1.000000000000000000 ) ) ;
#365 = DIRECTION ( 'NONE',  ( -8.911056267098788616E-18, -1.998401444326210262E-15, -1.000000000000000000 ) ) ;
#366 = ORIENTED_EDGE ( 'NONE', *, *, #16049, .T. ) ;
#367 = CARTESIAN_POINT ( 'NONE',  ( 6.272083055320289979, 16.72491874962310021, -5.657758596979629988E-15 ) ) ;
#368 = DESIGN_CONTEXT ( 'detailed design', #21695, 'design' ) ;
#369 = EDGE_CURVE ( 'NONE', #21866, #19301, #12226, .T. ) ;
#370 = PRODUCT_DEFINITION_SHAPE ( 'NONE', 'NONE',  #23499 ) ;
#371 = LOCAL_TIME ( 14, 11, 27.00000000000000000, #21009 ) ;
#372 = ORIENTED_EDGE ( 'NONE', *, *, #22651, .T. ) ;
#373 = ORIENTED_EDGE ( 'NONE', *, *, #19520, .F. ) ;
#374 = CARTESIAN_POINT ( 'NONE',  ( 34.41917370704140211, 26.49663125198719982, -20.00000000000029843 ) ) ;
#375 = DIRECTION ( 'NONE',  ( -3.210834492181040124E-17, 2.441916418604790135E-15, 1.000000000000000000 ) ) ;
#376 = AXIS2_PLACEMENT_3D ( 'NONE', #6732, #10429, #8275 ) ;
#377 = ORIENTED_EDGE ( 'NONE', *, *, #9879, .T. ) ;
#378 = CIRCLE ( 'NONE', #15561, 4.099999999999999645 ) ;
#379 = CARTESIAN_POINT ( 'NONE',  ( 32.14184541509679605, -2.767081550079640184, -13.00000000000039968 ) ) ;
#380 = CARTESIAN_POINT ( 'NONE',  ( -14.98746859791960162, 26.70208920133150343, 8.000000000004400036 ) ) ;
#381 = DATE_TIME_ROLE ( 'classification_date' ) ;
#382 = DIRECTION ( 'NONE',  ( -0.9730401042858024541, 0.2306359803922080898, 5.959266323858942451E-17 ) ) ;
#383 = AXIS2_PLACEMENT_3D ( 'NONE', #981, #4553, #22949 ) ;
#384 = ADVANCED_FACE ( 'NONE', ( #22889, #4726, #13202, #10087 ), #14970, .T. ) ;
#385 = EDGE_CURVE ( 'NONE', #9841, #20204, #20766, .T. ) ;
#386 = AXIS2_PLACEMENT_3D ( 'NONE', #4433, #11703, #4784 ) ;
#387 = DIRECTION ( 'NONE',  ( 2.199957270158029814E-13, -9.825194207785550278E-30, -1.000000000000000000 ) ) ;
#388 = CARTESIAN_POINT ( 'NONE',  ( 28.14554285793940025, -3.006546890859489896, 15.00000000000000000 ) ) ;
#389 = DATE_AND_TIME ( #9438, #17485 ) ;
#390 = LOCAL_TIME ( 14, 11, 27.00000000000000000, #15457 ) ;
#391 = APPROVAL_PERSON_ORGANIZATION ( #1848, #23135, #18023 ) ;
#392 = DIRECTION ( 'NONE',  ( -0.1997366180463769070, -0.8426774492125652660, 0.5000000000000002220 ) ) ;
#393 = DIRECTION ( 'NONE',  ( 0.1630842657209330415, 0.6880432561069529385, -0.7071067811865519026 ) ) ;
#394 = DIRECTION ( 'NONE',  ( -0.2306359803922009288, -0.9730401042858040084, 0.000000000000000000 ) ) ;
#395 = CYLINDRICAL_SURFACE ( 'NONE', #18197, 2.500000000000000888 ) ;
#396 = CARTESIAN_POINT ( 'NONE',  ( 32.12387896813558541, -7.901357381965649296, -13.00000000000000000 ) ) ;
#397 = DIRECTION ( 'NONE',  ( 1.000000000000000000, 1.829748171496159792E-16, 1.829748171496159792E-16 ) ) ;
#398 = CIRCLE ( 'NONE', #17469, 5.000000000000000888 ) ;
#399 = ORIENTED_EDGE ( 'NONE', *, *, #15334, .T. ) ;
#400 = EDGE_CURVE ( 'NONE', #9648, #22197, #1272, .T. ) ;
#401 = ORIENTED_EDGE ( 'NONE', *, *, #1811, .T. ) ;
#402 = CARTESIAN_POINT ( 'NONE',  ( -20.00000000397469790, 22.95208919256889857, -8.499999999995548450 ) ) ;
#403 = CARTESIAN_POINT ( 'NONE',  ( -25.00842861987479893, -15.87143667223269894, 25.00000000000000000 ) ) ;
#404 = VERTEX_POINT ( 'NONE', #8293 ) ;
#405 = DIRECTION ( 'NONE',  ( 0.000000000000000000, 1.000000000000000000, 0.000000000000000000 ) ) ;
#406 = ORIENTED_EDGE ( 'NONE', *, *, #6819, .F. ) ;
#407 = CC_DESIGN_APPROVAL ( #10855, ( #6120 ) ) ;
#408 = PLANE ( 'NONE',  #10336 ) ;
#409 = CC_DESIGN_APPROVAL ( #18154, ( #4599 ) ) ;
#410 = DATE_AND_TIME ( #18489, #16035 ) ;
#411 = DIRECTION ( 'NONE',  ( 0.000000000000000000, 0.000000000000000000, -1.000000000000000000 ) ) ;
#412 = EDGE_CURVE ( 'NONE', #11681, #1999, #22204, .T. ) ;
#413 = EDGE_CURVE ( 'NONE', #11749, #5148, #5943, .T. ) ;
#414 = APPROVAL_ROLE ( '' ) ;
#415 = DIRECTION ( 'NONE',  ( 1.000000000000000000, 0.000000000000000000, 0.000000000000000000 ) ) ;
#416 = CC_DESIGN_APPROVAL ( #4117, ( #8018 ) ) ;
#417 = FACE_OUTER_BOUND ( 'NONE', #3164, .T. ) ;
#418 = VERTEX_POINT ( 'NONE', #20437 ) ;
#419 = CARTESIAN_POINT ( 'NONE',  ( 30.89467803343008967, -3.022216679643965342, 15.00000000000011724 ) ) ;
#420 = ORIENTED_EDGE ( 'NONE', *, *, #158, .F. ) ;
#421 = DIRECTION ( 'NONE',  ( -1.000000000000000000, 0.000000000000000000, 0.000000000000000000 ) ) ;
#422 = APPROVAL_PERSON_ORGANIZATION ( #9790, #6450, #20927 ) ;
#423 = DIRECTION ( 'NONE',  ( 0.9286452767786566032, 1.871119812896368998E-17, -0.3709689338970208472 ) ) ;
#424 = ORIENTED_EDGE ( 'NONE', *, *, #14769, .F. ) ;
#425 = DIRECTION ( 'NONE',  ( 1.000000000000000000, -1.466984912809900042E-16, -5.345529420184390105E-52 ) ) ;
#427 = AXIS2_PLACEMENT_3D ( 'NONE', #20536, #16853, #578 ) ;
#426 = DIRECTION ( 'NONE',  ( -0.2306359803922085339, -0.9730401042858022320, 0.000000000000000000 ) ) ;
#428 = LINE ( 'NONE', #13156, #1760 ) ;
#429 = ORIENTED_EDGE ( 'NONE', *, *, #21082, .T. ) ;
#430 = AXIS2_PLACEMENT_3D ( 'NONE', #14037, #1324, #19618 ) ;
#431 = CARTESIAN_POINT ( 'NONE',  ( -30.79248430819439974, 6.338858557519089665, 2.999000000000090260 ) ) ;
#432 = LOCAL_TIME ( 14, 11, 27.00000000000000000, #4703 ) ;
#433 = ORIENTED_EDGE ( 'NONE', *, *, #10660, .T. ) ;
#434 = CC_DESIGN_PERSON_AND_ORGANIZATION_ASSIGNMENT ( #20935, #1093, ( #1104 ) ) ;
#435 = APPROVAL_ROLE ( '' ) ;
#436 = CARTESIAN_POINT ( 'NONE',  ( -0.5391976746782171093, 18.33937061236849075, -4.999999999999997335 ) ) ;
#437 = ORIENTED_EDGE ( 'NONE', *, *, #10962, .F. ) ;
#438 = ORIENTED_EDGE ( 'NONE', *, *, #17254, .F. ) ;
#439 = CARTESIAN_POINT ( 'NONE',  ( 43.98050001724080005, -5.573152644851309567, 15.50000000000019895 ) ) ;
#440 = DATE_TIME_ROLE ( 'classification_date' ) ;
#441 = LOCAL_TIME ( 14, 11, 27.00000000000000000, #15823 ) ;
#442 = PERSON_AND_ORGANIZATION ( #18147, #21281 ) ;
#443 = DIRECTION ( 'NONE',  ( 6.009176021521548497E-19, -0.9999588795606766389, -0.009068582455715215943 ) ) ;
#444 = VECTOR ( 'NONE', #7289, 1000.000000000000000 ) ;
#445 = AXIS2_PLACEMENT_3D ( 'NONE', #15992, #21341, #4955 ) ;
#446 = APPROVAL_PERSON_ORGANIZATION ( #1014, #12836, #19205 ) ;
#447 = DIRECTION ( 'NONE',  ( -0.7070970883417647679, -0.003702385528188428636, -0.7071067811865467956 ) ) ;
#448 = AXIS2_PLACEMENT_3D ( 'NONE', #2877, #8220, #22687 ) ;
#449 = EDGE_CURVE ( 'NONE', #23261, #20507, #13870, .T. ) ;
#450 = DATE_TIME_ROLE ( 'classification_date' ) ;
#451 = AXIS2_PLACEMENT_3D ( 'NONE', #12252, #19482, #8439 ) ;
#452 = ORIENTED_EDGE ( 'NONE', *, *, #18200, .T. ) ;
#453 = DIRECTION ( 'NONE',  ( -0.005235963827108352890, 0.9999862922474493931, 5.936218956694023463E-19 ) ) ;
#454 = ORIENTED_EDGE ( 'NONE', *, *, #21393, .F. ) ;
#455 = CC_DESIGN_APPROVAL ( #7933, ( #8830 ) ) ;
#456 = CARTESIAN_POINT ( 'NONE',  ( 61.93563330948220624, 19.01565939351212009, -13.00000000000000000 ) ) ;
#457 = DIRECTION ( 'NONE',  ( 0.9730401042858035643, -0.2306359803922028717, 2.025546614365803772E-16 ) ) ;
#458 = CARTESIAN_POINT ( 'NONE',  ( 37.91003399039541222, 9.225896048119837545, -26.88000000000049639 ) ) ;
#459 = ORIENTED_EDGE ( 'NONE', *, *, #16927, .F. ) ;
#460 = EDGE_LOOP ( 'NONE', ( #10662, #7754 ) ) ;
#461 = CARTESIAN_POINT ( 'NONE',  ( -62.75934763415060047, -21.57895147295310068, -5.536226058455569256E-15 ) ) ;
#462 = AXIS2_PLACEMENT_3D ( 'NONE', #21262, #17608, #4890 ) ;
#463 = EDGE_LOOP ( 'NONE', ( #7815, #9677, #22986, #7812 ) ) ;
#464 = AXIS2_PLACEMENT_3D ( 'NONE', #6114, #639, #2555 ) ;
#465 = EDGE_CURVE ( 'NONE', #2857, #7141, #671, .T. ) ;
#466 = CALENDAR_DATE ( 2026, 31, 10 ) ;
#467 = VERTEX_POINT ( 'NONE', #8539 ) ;
#468 = AXIS2_PLACEMENT_3D ( 'NONE', #6607, #22852, #3255 ) ;
#469 = ORIENTED_EDGE ( 'NONE', *, *, #21827, .F. ) ;
#470 = DIRECTION ( 'NONE',  ( -0.9997648975362233292, -0.02168293463498000007, 0.000000000000000000 ) ) ;
#471 = DIRECTION ( 'NONE',  ( 0.000000000000000000, 1.000000000000000000, 0.000000000000000000 ) ) ;
#472 = PERSON_AND_ORGANIZATION_ROLE ( 'creator' ) ;
#473 = APPLICATION_CONTEXT ( 'configuration controlled 3d designs of mechanical parts and assemblies' ) ;
#474 = DIRECTION ( 'NONE',  ( -1.138590270679734009E-14, -2.220446049251240387E-15, -1.000000000000000000 ) ) ;
#475 = VECTOR ( 'NONE', #6240, 1000.000000000000000 ) ;
#476 = EDGE_CURVE ( 'NONE', #6299, #3647, #15768, .T. ) ;
#477 = FACE_OUTER_BOUND ( 'NONE', #722, .T. ) ;
#478 = AXIS2_PLACEMENT_3D ( 'NONE', #21824, #14241, #10702 ) ;
#479 = AXIS2_PLACEMENT_3D ( 'NONE', #2013, #5569, #16719 ) ;
#480 = SECURITY_CLASSIFICATION ( '', '', #9819 ) ;
#481 =( NAMED_UNIT ( * ) SI_UNIT ( $, .STERADIAN. ) SOLID_ANGLE_UNIT ( ) );
#482 = CIRCLE ( 'NONE', #15677, 2.499999999999998668 ) ;
#483 = VERTEX_POINT ( 'NONE', #6751 ) ;
#484 = CARTESIAN_POINT ( 'NONE',  ( -11.24263882182209962, 20.87636639668270178, -2.982050098520939832E-15 ) ) ;
#485 = ADVANCED_FACE ( 'NONE', ( #13983 ), #21215, .F. ) ;
#486 = MECHANICAL_CONTEXT ( 'NONE', #13521, 'mechanical' ) ;
#487 = AXIS2_PLACEMENT_3D ( 'NONE', #6092, #13572, #13346 ) ;
#488 = SHAPE_REPRESENTATION ( '1602p_c_17', ( #12739 ), #13514 ) ;
#489 = VERTEX_POINT ( 'NONE', #1847 ) ;
#490 = LINE ( 'NONE', #2631, #20485 ) ;
#491 = FACE_OUTER_BOUND ( 'NONE', #938, .T. ) ;
#492 = EDGE_LOOP ( 'NONE', ( #9352, #22717 ) ) ;
#493 = CC_DESIGN_DATE_AND_TIME_ASSIGNMENT ( #1620, #14334, ( #62 ) ) ;
#494 = CARTESIAN_POINT ( 'NONE',  ( 52.49909637502329929, -7.592283011512489743, 15.25462000000019991 ) ) ;
#495 = DIRECTION ( 'NONE',  ( -2.979590041760124764E-09, 0.4472135954999595375, -0.8944271909999150783 ) ) ;
#496 = EDGE_LOOP ( 'NONE', ( #15105, #1345 ) ) ;
#497 = PLANE ( 'NONE',  #847 ) ;
#498 = EDGE_CURVE ( 'NONE', #6410, #20342, #16990, .T. ) ;
#499 = EDGE_CURVE ( 'NONE', #16530, #2857, #12789, .T. ) ;
#500 = CALENDAR_DATE ( 2026, 31, 10 ) ;
#501 = SHAPE_DEFINITION_REPRESENTATION ( #22718, #9605 ) ;
#502 = CONICAL_SURFACE ( 'NONE', #13794, 5.086751345948125724, 1.047197551196598297 ) ;
#503 = VERTEX_POINT ( 'NONE', #20025 ) ;
#504 = ORIENTED_EDGE ( 'NONE', *, *, #16314, .F. ) ;
#505 = LINE ( 'NONE', #20807, #5051 ) ;
#506 = CARTESIAN_POINT ( 'NONE',  ( 36.09092202081949807, 8.115512906978191054, -29.25000000000050093 ) ) ;
#507 = ORIENTED_EDGE ( 'NONE', *, *, #19720, .T. ) ;
#508 = AXIS2_PLACEMENT_3D ( 'NONE', #18123, #10789, #12884 ) ;
#509 = PERSON_AND_ORGANIZATION ( #11966, #8758 ) ;
#510 = LINE ( 'NONE', #10617, #19480 ) ;
#511 = CIRCLE ( 'NONE', #17976, 2.499999999999999112 ) ;
#512 = CARTESIAN_POINT ( 'NONE',  ( 2.664535259100379799E-14, -1.554450629062440126E-15, 2.500000000000000000 ) ) ;
#513 = SECURITY_CLASSIFICATION_LEVEL ( 'unclassified' ) ;
#514 = DIRECTION ( 'NONE',  ( 1.138590270679730064E-14, 2.220446049251240387E-15, 1.000000000000000000 ) ) ;
#515 = FACE_OUTER_BOUND ( 'NONE', #10689, .T. ) ;
#516 = DIRECTION ( 'NONE',  ( -0.1630842657209334579, -0.6880432561069538266, 0.7071067811865507924 ) ) ;
#517 = EDGE_CURVE ( 'NONE', #3272, #20682, #5535, .T. ) ;
#518 = DATE_AND_TIME ( #11241, #15953 ) ;
#519 = VECTOR ( 'NONE', #21542, 1000.000000000000000 ) ;
#520 = DIRECTION ( 'NONE',  ( 0.000000000000000000, 0.000000000000000000, 1.000000000000000000 ) ) ;
#521 = CIRCLE ( 'NONE', #4340, 4.999999999999995559 ) ;
#522 = DIRECTION ( 'NONE',  ( 0.000000000000000000, 1.734723475976806848E-16, 1.000000000000000000 ) ) ;
#523 = CC_DESIGN_PERSON_AND_ORGANIZATION_ASSIGNMENT ( #8787, #12369, ( #5042 ) ) ;
#524 = DIRECTION ( 'NONE',  ( -0.9730401042858035643, 0.2306359803922031215, 0.000000000000000000 ) ) ;
#525 = DIRECTION ( 'NONE',  ( -1.751019220569994795E-16, -2.300154215587015208E-15, -1.000000000000000000 ) ) ;
#526 = CC_DESIGN_DATE_AND_TIME_ASSIGNMENT ( #7605, #16862, ( #16700 ) ) ;
#527 = CARTESIAN_POINT ( 'NONE',  ( -2.966462739374829791E-16, -7.772954297906289827E-16, -2.500000000000090150 ) ) ;
#528 = CARTESIAN_POINT ( 'NONE',  ( 5.000000000000000000, -31.09999999999999787, -6.250000000000000000 ) ) ;
#529 = EDGE_CURVE ( 'NONE', #10876, #12306, #23421, .T. ) ;
#531 = EDGE_LOOP ( 'NONE', ( #9595, #23275, #15737, #7809 ) ) ;
#530 = EDGE_CURVE ( 'NONE', #16237, #5287, #3326, .T. ) ;
#532 = EDGE_LOOP ( 'NONE', ( #10638, #21531, #13593, #19724 ) ) ;
#533 = DIRECTION ( 'NONE',  ( -1.000000000000000000, 0.000000000000000000, 0.000000000000000000 ) ) ;
#534 = DIRECTION ( 'NONE',  ( 0.9730401042858036753, -0.2306359803922031493, -5.432877459303553216E-17 ) ) ;
#535 = ADVANCED_FACE ( 'NONE', ( #23459 ), #3525, .T. ) ;
#536 = ORIENTED_EDGE ( 'NONE', *, *, #21834, .F. ) ;
#537 = LINE ( 'NONE', #4699, #2759 ) ;
#538 = ORIENTED_EDGE ( 'NONE', *, *, #17504, .F. ) ;
#539 = CARTESIAN_POINT ( 'NONE',  ( 6.500000000000000000, -17.30000000000000071, -2.500000000000000000 ) ) ;
#540 = COORDINATED_UNIVERSAL_TIME_OFFSET ( 0, 0, .AHEAD. ) ;
#541 = CARTESIAN_POINT ( 'NONE',  ( -70.63306599754589854, 6.130251853413639651, -3.000000000000079936 ) ) ;
#542 = SECURITY_CLASSIFICATION_LEVEL ( 'unclassified' ) ;
#543 = CARTESIAN_POINT ( 'NONE',  ( 62.20574963825990267, 1.227340145578230013, 4.500000000000000000 ) ) ;
#544 = VERTEX_POINT ( 'NONE', #12446 ) ;
#545 = EDGE_CURVE ( 'NONE', #3168, #668, #1035, .T. ) ;
#546 = CARTESIAN_POINT ( 'NONE',  ( 113.2033677465029911, -29.17473274740290279, -3.099999999999920153 ) ) ;
#547 = VERTEX_POINT ( 'NONE', #14221 ) ;
#548 = DIRECTION ( 'NONE',  ( -0.000000000000000000, -0.000000000000000000, 1.000000000000000000 ) ) ;
#549 = EDGE_CURVE ( 'NONE', #20086, #18306, #5988, .T. ) ;
#550 = CARTESIAN_POINT ( 'NONE',  ( 33.37436288052550282, -3.059220458576299873, 13.00000000000019895 ) ) ;
#551 = VERTEX_POINT ( 'NONE', #15995 ) ;
#552 = FACE_OUTER_BOUND ( 'NONE', #15319, .T. ) ;
#553 = LINE ( 'NONE', #20395, #17489 ) ;
#554 = VERTEX_POINT ( 'NONE', #18139 ) ;
#555 = EDGE_CURVE ( 'NONE', #17008, #6563, #19274, .T. ) ;
#556 = AXIS2_PLACEMENT_3D ( 'NONE', #1022, #22638, #22995 ) ;
#557 = CONTEXT_DEPENDENT_SHAPE_REPRESENTATION ( #12507, #18611 ) ;
#558 = EDGE_CURVE ( 'NONE', #21066, #22882, #12087, .T. ) ;
#559 = LINE ( 'NONE', #17060, #5451 ) ;
#560 = VERTEX_POINT ( 'NONE', #19918 ) ;
#561 = PERSON_AND_ORGANIZATION ( #11966, #8758 ) ;
#562 = DIRECTION ( 'NONE',  ( 0.2306359803922080898, 0.9730401042858024541, -2.572202231434325988E-16 ) ) ;
#563 = VERTEX_POINT ( 'NONE', #6998 ) ;
#564 = ORIENTED_EDGE ( 'NONE', *, *, #13143, .F. ) ;
#565 = DIRECTION ( 'NONE',  ( 0.9730401042858036753, -0.2306359803922028995, -5.432877459303547669E-17 ) ) ;
#566 = APPLICATION_PROTOCOL_DEFINITION ( 'international standard', 'config_control_design', 1994, #1690 ) ;
#567 = ADVANCED_BREP_SHAPE_REPRESENTATION ( '', ( #1705, #12739 ), #22737 ) ;
#568 = AXIS2_PLACEMENT_3D ( 'NONE', #4257, #18774, #20648 ) ;
#569 = APPROVAL_DATE_TIME ( #20756, #1502 ) ;
#570 = CARTESIAN_POINT ( 'NONE',  ( 113.9239269372040013, -8.791386740117969723, 3.438967838479089450E-14 ) ) ;
#571 = DIRECTION ( 'NONE',  ( 1.000000000000000000, 0.000000000000000000, 0.000000000000000000 ) ) ;
#572 = CARTESIAN_POINT ( 'NONE',  ( 35.59419854219520118, 9.774809681453518806, 19.56700000000000017 ) ) ;
#573 = EDGE_LOOP ( 'NONE', ( #11561, #21123, #806, #4232, #14126, #5854, #13368 ) ) ;
#574 = APPROVAL ( #3213, 'UNSPECIFIED' ) ;
#575 = APPROVAL_STATUS ( 'not_yet_approved' ) ;
#576 = PRODUCT ( '1602p_c_14', '1602p_c_14', '', ( #2740 ) ) ;
#577 = VERTEX_POINT ( 'NONE', #21676 ) ;
#578 = DIRECTION ( 'NONE',  ( -0.2306359803922033158, -0.9730401042858034533, 0.000000000000000000 ) ) ;
#579 = ORIENTED_EDGE ( 'NONE', *, *, #4356, .F. ) ;
#580 = CARTESIAN_POINT ( 'NONE',  ( 27.73073027566755044, -1.721531772301079899, -13.00000000000000000 ) ) ;
#581 = AXIS2_PLACEMENT_3D ( 'NONE', #2091, #6128, #20273 ) ;
#582 = CARTESIAN_POINT ( 'NONE',  ( 113.4570673249340018, -28.10438863268850085, -3.399999999999949729 ) ) ;
#583 = CARTESIAN_POINT ( 'NONE',  ( -6.134178274321590685, 19.66552749962360025, -1.543041128605420056E-15 ) ) ;
#584 = EDGE_LOOP ( 'NONE', ( #9967, #15754, #19840, #6241, #22801 ) ) ;
#585 = ORIENTED_EDGE ( 'NONE', *, *, #14857, .F. ) ;
#586 = CARTESIAN_POINT ( 'NONE',  ( 33.27705887009660302, -3.036156860536515012, 13.00000000000000000 ) ) ;
#587 = VERTEX_POINT ( 'NONE', #21457 ) ;
#588 = CALENDAR_DATE ( 2026, 31, 10 ) ;
#589 = CIRCLE ( 'NONE', #12378, 2.499999999999999112 ) ;
#590 = ORIENTED_EDGE ( 'NONE', *, *, #8239, .F. ) ;
#591 = ORIENTED_EDGE ( 'NONE', *, *, #15449, .T. ) ;
#592 = DIRECTION ( 'NONE',  ( -0.005235963827121941846, 0.9999862922474492821, 5.936218956657112052E-19 ) ) ;
#593 = PERSON_AND_ORGANIZATION_ROLE ( 'design_owner' ) ;
#594 = CARTESIAN_POINT ( 'NONE',  ( -66.29618031796869104, -0.3471291603817610039, -3.000000000000079936 ) ) ;
#595 = EDGE_CURVE ( 'NONE', #21743, #4396, #5423, .T. ) ;
#596 = CARTESIAN_POINT ( 'NONE',  ( 2.671834669462799905, 17.57827187707419725, 5.250000012366680124 ) ) ;
#597 = ORIENTED_EDGE ( 'NONE', *, *, #2152, .F. ) ;
#598 = CIRCLE ( 'NONE', #13894, 3.499999999999998224 ) ;
#599 = CARTESIAN_POINT ( 'NONE',  ( -2.384285517815838862, 10.55504977808206846, -9.087704672992351837E-16 ) ) ;
#600 = APPROVAL_DATE_TIME ( #133, #2186 ) ;
#601 = ORIENTED_EDGE ( 'NONE', *, *, #16837, .F. ) ;
#602 = LINE ( 'NONE', #4309, #22373 ) ;
#603 = DIRECTION ( 'NONE',  ( 0.9730401042858035643, -0.2306359803922031215, 2.804983810440351899E-16 ) ) ;
#604 = ORIENTED_EDGE ( 'NONE', *, *, #13332, .T. ) ;
#605 = CARTESIAN_POINT ( 'NONE',  ( -27.00000000000000000, -28.60000000000000142, -2.500000000000000000 ) ) ;
#606 = ORIENTED_EDGE ( 'NONE', *, *, #3941, .F. ) ;
#607 = DIRECTION ( 'NONE',  ( 0.002617981913558544045, -0.4999931461237241970, 0.8660254037844389297 ) ) ;
#608 = APPLICATION_CONTEXT ( 'configuration controlled 3d designs of mechanical parts and assemblies' ) ;
#609 = PERSON_AND_ORGANIZATION_ROLE ( 'creator' ) ;
#610 = CIRCLE ( 'NONE', #16928, 2.066999999999999726 ) ;
#611 = ORIENTED_EDGE ( 'NONE', *, *, #216, .F. ) ;
#612 = ORIENTED_EDGE ( 'NONE', *, *, #6730, .F. ) ;
#613 = CARTESIAN_POINT ( 'NONE',  ( 31.01827548281339020, -2.500766059351137827, -15.00000000000039613 ) ) ;
#614 = AXIS2_PLACEMENT_3D ( 'NONE', #10276, #10510, #19288 ) ;
#615 = CYLINDRICAL_SURFACE ( 'NONE', #9091, 2.499999999999999112 ) ;
#616 = ORIENTED_EDGE ( 'NONE', *, *, #17227, .T. ) ;
#617 = DATE_AND_TIME ( #9907, #3100 ) ;
#618 = DIRECTION ( 'NONE',  ( 0.000000000000000000, 0.000000000000000000, 1.000000000000000000 ) ) ;
#619 = EDGE_CURVE ( 'NONE', #14838, #21047, #1807, .T. ) ;
#620 = DIRECTION ( 'NONE',  ( 0.2306359803922031215, 0.9730401042858034533, -4.741332172907939802E-18 ) ) ;
#621 = CALENDAR_DATE ( 2026, 31, 10 ) ;
#622 = CARTESIAN_POINT ( 'NONE',  ( 52.49909637502329929, -7.592283011512489743, 13.00000000000019895 ) ) ;
#623 =( BOUNDED_CURVE ( )  B_SPLINE_CURVE ( 2, ( #18921, #2420, #613 ),
 .UNSPECIFIED., .F., .F. ) 
 B_SPLINE_CURVE_WITH_KNOTS ( ( 3, 3 ),
 ( 0.000000000000000000, 0.1168436138077930952 ),
 .UNSPECIFIED. ) 
 CURVE ( )  GEOMETRIC_REPRESENTATION_ITEM ( )  RATIONAL_B_SPLINE_CURVE ( ( 1.000000000000000000, 1.077350269189630172, 1.077350269189629950 ) ) 
 REPRESENTATION_ITEM ( '' )  );
#624 = DIRECTION ( 'NONE',  ( 0.2306359803922030383, 0.9730401042858035643, -1.407521210652539229E-17 ) ) ;
#625 = ADVANCED_FACE ( 'NONE', ( #1615 ), #14571, .T. ) ;
#626 = EDGE_CURVE ( 'NONE', #15831, #13288, #12347, .T. ) ;
#627 = CARTESIAN_POINT ( 'NONE',  ( -62.73971250800079957, -25.32895006819559924, -5.000000000000000000 ) ) ;
#628 = PERSON_AND_ORGANIZATION ( #11966, #8758 ) ;
#629 = AXIS2_PLACEMENT_3D ( 'NONE', #2608, #14751, #21978 ) ;
#630 = AXIS2_PLACEMENT_3D ( 'NONE', #10750, #19876, #18085 ) ;
#631 = CARTESIAN_POINT ( 'NONE',  ( -67.10797875267205370, -21.85177448797741917, -6.069095851239679835E-15 ) ) ;
#632 = DIRECTION ( 'NONE',  ( -1.085472681297010170E-15, -4.321163532573060300E-15, -1.000000000000000000 ) ) ;
#633 = CARTESIAN_POINT ( 'NONE',  ( 34.40839383886530101, 23.41606575285529956, 13.00000000000000000 ) ) ;
#634 = CYLINDRICAL_SURFACE ( 'NONE', #20520, 5.000000000000001776 ) ;
#635 = DIRECTION ( 'NONE',  ( 1.138590270679730064E-14, 2.220446049251235259E-15, 1.000000000000000000 ) ) ;
#636 = LINE ( 'NONE', #7897, #13374 ) ;
#637 = ORIENTED_EDGE ( 'NONE', *, *, #4722, .T. ) ;
#638 = VERTEX_POINT ( 'NONE', #16114 ) ;
#639 = DIRECTION ( 'NONE',  ( -2.269747459788999852E-13, -2.220446049250320181E-15, -1.000000000000000000 ) ) ;
#640 = CARTESIAN_POINT ( 'NONE',  ( 118.6002496876800052, -6.405594307115060282, 15.90000000000000036 ) ) ;
#641 = VECTOR ( 'NONE', #20224, 1000.000000000000000 ) ;
#642 = ORIENTED_EDGE ( 'NONE', *, *, #16160, .T. ) ;
#643 = CARTESIAN_POINT ( 'NONE',  ( -25.44812980900369936, 25.46511081327010118, 2.499999999999940048 ) ) ;
#644 = EDGE_CURVE ( 'NONE', #13133, #11391, #14330, .T. ) ;
#645 = VERTEX_POINT ( 'NONE', #21913 ) ;
#646 = CIRCLE ( 'NONE', #9006, 2.499999999999999112 ) ;
#647 = DIRECTION ( 'NONE',  ( 2.269747459788994803E-13, 2.220446049250715400E-15, 1.000000000000000000 ) ) ;
#648 = VECTOR ( 'NONE', #22926, 999.9999999999998863 ) ;
#649 = APPROVAL_ROLE ( '' ) ;
#650 = CARTESIAN_POINT ( 'NONE',  ( 43.84419854219520829, -31.09999999999999787, -21.50000000000000000 ) ) ;
#651 = APPROVAL ( #15739, 'UNSPECIFIED' ) ;
#652 = CC_DESIGN_DATE_AND_TIME_ASSIGNMENT ( #15164, #8054, ( #6120 ) ) ;
#653 = CONTEXT_DEPENDENT_SHAPE_REPRESENTATION ( #16893, #20100 ) ;
#654 =( REPRESENTATION_RELATIONSHIP ('NONE','NONE', #18771, #15964 ) REPRESENTATION_RELATIONSHIP_WITH_TRANSFORMATION ( #7645 )SHAPE_REPRESENTATION_RELATIONSHIP( ) );
#655 = DIRECTION ( 'NONE',  ( -0.9730401042858036753, 0.2306359803922028995, -2.804983810440358801E-16 ) ) ;
#656 = ADVANCED_FACE ( 'NONE', ( #11261 ), #13251, .F. ) ;
#657 = EDGE_CURVE ( 'NONE', #23364, #20134, #2455, .T. ) ;
#658 = ORIENTED_EDGE ( 'NONE', *, *, #17806, .F. ) ;
#659 = APPROVAL ( #2364, 'UNSPECIFIED' ) ;
#660 = VECTOR ( 'NONE', #10249, 1000.000000000000000 ) ;
#661 = EDGE_LOOP ( 'NONE', ( #8314, #14025 ) ) ;
#662 = FACE_OUTER_BOUND ( 'NONE', #16612, .T. ) ;
#663 = DIRECTION ( 'NONE',  ( 0.9730401042858035643, -0.2306359803922028717, -5.432877459303547053E-17 ) ) ;
#664 = VECTOR ( 'NONE', #5401, 1000.000000000000114 ) ;
#665 = ORIENTED_EDGE ( 'NONE', *, *, #2304, .F. ) ;
#666 = LINE ( 'NONE', #4365, #15048 ) ;
#667 = FACE_OUTER_BOUND ( 'NONE', #10413, .T. ) ;
#668 = VERTEX_POINT ( 'NONE', #7792 ) ;
#669 = ITEM_DEFINED_TRANSFORMATION ( 'NONE', 'NONE', #6831,  #12739 ) ;
#670 = DIRECTION ( 'NONE',  ( 0.2306359803922019280, 0.9730401042858037863, -1.407521210652539229E-17 ) ) ;
#671 = CIRCLE ( 'NONE', #7138, 2.499999999999998668 ) ;
#672 = ORIENTED_EDGE ( 'NONE', *, *, #10946, .T. ) ;
#673 = COORDINATED_UNIVERSAL_TIME_OFFSET ( 0, 0, .AHEAD. ) ;
#674 = CARTESIAN_POINT ( 'NONE',  ( 2.018067881930598162, 20.45665492794147866, -6.773018412508057079E-15 ) ) ;
#675 = EDGE_CURVE ( 'NONE', #16036, #9718, #15138, .T. ) ;
#676 = ORIENTED_EDGE ( 'NONE', *, *, #8180, .T. ) ;
#677 = VERTEX_POINT ( 'NONE', #6121 ) ;
#678 = PLANE ( 'NONE',  #14136 ) ;
#679 = VECTOR ( 'NONE', #9754, 1000.000000000000000 ) ;
#680 = APPLICATION_PROTOCOL_DEFINITION ( 'international standard', 'config_control_design', 1994, #17476 ) ;
#681 = CALENDAR_DATE ( 2026, 31, 10 ) ;
#682 = AXIS2_PLACEMENT_3D ( 'NONE', #22326, #20327, #20442 ) ;
#683 = DIRECTION ( 'NONE',  ( -1.000000000000000000, 0.000000000000000000, 0.000000000000000000 ) ) ;
#684 = EDGE_CURVE ( 'NONE', #2339, #15644, #6765, .T. ) ;
#685 = ADVANCED_FACE ( 'NONE', ( #2454 ), #9804, .T. ) ;
#686 = DIRECTION ( 'NONE',  ( 0.9822618273148069346, -0.1875145397033960160, 4.933538860811973842E-16 ) ) ;
#687 = VERTEX_POINT ( 'NONE', #5647 ) ;
#688 = CALENDAR_DATE ( 2026, 31, 10 ) ;
#689 = ORIENTED_EDGE ( 'NONE', *, *, #9412, .F. ) ;
#690 = LINE ( 'NONE', #3920, #15989 ) ;
#691 = CARTESIAN_POINT ( 'NONE',  ( -17.50000000000000000, -20.00000000000000000, 0.000000000000000000 ) ) ;
#692 = ORIENTED_EDGE ( 'NONE', *, *, #5300, .T. ) ;
#693 = FACE_OUTER_BOUND ( 'NONE', #12076, .T. ) ;
#695 = VECTOR ( 'NONE', #13903, 1000.000000000000000 ) ;
#694 = CARTESIAN_POINT ( 'NONE',  ( 35.59419854219520118, 9.774809681453239918, -37.44562646538079775 ) ) ;
#696 = CARTESIAN_POINT ( 'NONE',  ( 33.27705887009660302, -3.036156860536499913, 13.00000000000000000 ) ) ;
#697 = ORIENTED_EDGE ( 'NONE', *, *, #6201, .T. ) ;
#698 = ORIENTED_EDGE ( 'NONE', *, *, #20723, .T. ) ;
#699 = CARTESIAN_POINT ( 'NONE',  ( -20.00000000397369959, 22.95208919256949898, -3.750000000000059508 ) ) ;
#700 = EDGE_LOOP ( 'NONE', ( #22607, #4865 ) ) ;
#701 = APPROVAL_STATUS ( 'not_yet_approved' ) ;
#702 = EDGE_LOOP ( 'NONE', ( #22974, #1504 ) ) ;
#703 = ORIENTED_EDGE ( 'NONE', *, *, #8835, .F. ) ;
#704 = DIRECTION ( 'NONE',  ( 0.000000000000000000, 1.020425574104004122E-16, 1.000000000000000000 ) ) ;
#705 = COORDINATED_UNIVERSAL_TIME_OFFSET ( 0, 0, .AHEAD. ) ;
#706 = DIRECTION ( 'NONE',  ( -6.662161100567945949E-09, 1.000000000000000000, -2.220444537107962377E-15 ) ) ;
#707 = ADVANCED_FACE ( 'NONE', ( #3989 ), #12448, .T. ) ;
#708 = LINE ( 'NONE', #17109, #7822 ) ;
#709 = EDGE_CURVE ( 'NONE', #4115, #1299, #12822, .T. ) ;
#710 = APPROVAL_ROLE ( '' ) ;
#711 = EDGE_LOOP ( 'NONE', ( #16585, #16731 ) ) ;
#712 = APPROVAL_PERSON_ORGANIZATION ( #204, #10254, #16487 ) ;
#713 = CARTESIAN_POINT ( 'NONE',  ( -59.07950864401301772, -25.30978511045550050, 3.660254037844370423 ) ) ;
#714 = CIRCLE ( 'NONE', #20466, 2.749999999999999112 ) ;
#715 = CARTESIAN_POINT ( 'NONE',  ( -19.99999999999849720, -20.00000000000000000, 6.500000000004389378 ) ) ;
#716 = ORIENTED_EDGE ( 'NONE', *, *, #13563, .T. ) ;
#717 = DIRECTION ( 'NONE',  ( -0.2306359803922010121, -0.9730401042858040084, 0.000000000000000000 ) ) ;
#718 = DIRECTION ( 'NONE',  ( 6.281952996264450405E-17, 4.969341027148649850E-15, 1.000000000000000000 ) ) ;
#719 = VERTEX_POINT ( 'NONE', #5890 ) ;
#720 = DIRECTION ( 'NONE',  ( 5.810967191216043342E-28, 4.938475297218040001E-14, 1.000000000000000000 ) ) ;
#721 = CALENDAR_DATE ( 2026, 31, 10 ) ;
#722 = EDGE_LOOP ( 'NONE', ( #3744, #4350 ) ) ;
#723 = EDGE_LOOP ( 'NONE', ( #14438, #13051, #6044, #8193, #9529, #11889, #19904, #12108, #1672, #3809, #15184, #2137, #14325, #14667 ) ) ;
#724 = DIRECTION ( 'NONE',  ( -0.9997648975362221080, -0.02168293463503390486, 0.000000000000000000 ) ) ;
#725 = DIRECTION ( 'NONE',  ( 0.9822618273148069346, -0.1875145397033960160, 4.845439952583188648E-16 ) ) ;
#726 = PLANE ( 'NONE',  #19683 ) ;
#727 = CALENDAR_DATE ( 2026, 31, 10 ) ;
#728 = CARTESIAN_POINT ( 'NONE',  ( -27.00000000000000000, -31.09999999999999787, -6.250000000000000000 ) ) ;
#729 = DIRECTION ( 'NONE',  ( -0.9730401042858022320, 0.2306359803922080343, 8.445809534385342559E-31 ) ) ;
#730 = DATE_AND_TIME ( #5867, #7716 ) ;
#731 = CIRCLE ( 'NONE', #13652, 2.750000000000001332 ) ;
#732 = FACE_OUTER_BOUND ( 'NONE', #3446, .T. ) ;
#733 = VECTOR ( 'NONE', #8527, 999.9999999999998863 ) ;
#734 = CYLINDRICAL_SURFACE ( 'NONE', #5234, 6.499999999999997335 ) ;
#735 = SECURITY_CLASSIFICATION_LEVEL ( 'unclassified' ) ;
#736 = CARTESIAN_POINT ( 'NONE',  ( 37.48968750243700043, 22.68571848161319693, -13.00000000000049916 ) ) ;
#737 = DIRECTION ( 'NONE',  ( -0.9730401042858036753, 0.2306359803922028995, 5.958148513035547083E-17 ) ) ;
#738 = EDGE_CURVE ( 'NONE', #12414, #131, #2184, .T. ) ;
#739 = CARTESIAN_POINT ( 'NONE',  ( -19.81505072009858992, 25.44523855881121577, -4.999999999995566213 ) ) ;
#740 = EDGE_CURVE ( 'NONE', #9811, #6317, #14408, .T. ) ;
#741 = LOCAL_TIME ( 14, 11, 27.00000000000000000, #3778 ) ;
#742 = CARTESIAN_POINT ( 'NONE',  ( -19.49999999982360066, -0.1021026942259700004, 2.500000000000000000 ) ) ;
#743 =( GEOMETRIC_REPRESENTATION_CONTEXT ( 3 ) GLOBAL_UNCERTAINTY_ASSIGNED_CONTEXT ( ( #2693 ) ) GLOBAL_UNIT_ASSIGNED_CONTEXT ( ( #14712, #21941, #12932 ) ) REPRESENTATION_CONTEXT ( 'NONE', 'WORKASPACE' ) );
#744 = AXIS2_PLACEMENT_3D ( 'NONE', #21021, #1047, #4747 ) ;
#745 = CARTESIAN_POINT ( 'NONE',  ( -22.50000000000000000, -20.00000001665527805, 5.500000000004588330 ) ) ;
#746 = VERTEX_POINT ( 'NONE', #11500 ) ;
#747 = VERTEX_POINT ( 'NONE', #18608 ) ;
#748 = FACE_OUTER_BOUND ( 'NONE', #10952, .T. ) ;
#749 = CARTESIAN_POINT ( 'NONE',  ( 39.27359436029429673, 22.26288585089429972, 13.00000000000000000 ) ) ;
#750 = ORIENTED_EDGE ( 'NONE', *, *, #5274, .F. ) ;
#751 = VECTOR ( 'NONE', #11337, 1000.000000000000000 ) ;
#752 = EDGE_CURVE ( 'NONE', #10345, #1222, #13375, .T. ) ;
#753 = CARTESIAN_POINT ( 'NONE',  ( -16.00004797695772751, -0.08377682083104273647, -8.699586588110780178E-14 ) ) ;
#754 = ORIENTED_EDGE ( 'NONE', *, *, #12897, .F. ) ;
#755 = FACE_OUTER_BOUND ( 'NONE', #14144, .T. ) ;
#756 =( BOUNDED_CURVE ( )  B_SPLINE_CURVE ( 2, ( #16512, #234, #2624 ),
 .UNSPECIFIED., .F., .F. ) 
 B_SPLINE_CURVE_WITH_KNOTS ( ( 3, 3 ),
 ( 0.000000000000000000, 0.2336872276155859962 ),
 .UNSPECIFIED. ) 
 CURVE ( )  GEOMETRIC_REPRESENTATION_ITEM ( )  RATIONAL_B_SPLINE_CURVE ( ( 1.000000000000000000, 1.154700538379259900, 1.000000000000000000 ) ) 
 REPRESENTATION_ITEM ( '' )  );
#757 = AXIS2_PLACEMENT_3D ( 'NONE', #19049, #10151, #729 ) ;
#758 = APPROVAL_STATUS ( 'not_yet_approved' ) ;
#759 = FACE_OUTER_BOUND ( 'NONE', #8921, .T. ) ;
#760 = PRODUCT_DEFINITION_SHAPE ( 'NONE', 'NONE',  #23486 ) ;
#761 = CC_DESIGN_APPROVAL ( #10128, ( #21633 ) ) ;
#762 = COORDINATED_UNIVERSAL_TIME_OFFSET ( 0, 0, .AHEAD. ) ;
#763 = DIRECTION ( 'NONE',  ( 0.1997366180463774621, 0.8426774492125632676, -0.5000000000000035527 ) ) ;
#764 = AXIS2_PLACEMENT_3D ( 'NONE', #12664, #23325, #17877 ) ;
#765 = DIRECTION ( 'NONE',  ( -1.000000000000000000, 0.000000000000000000, -3.099353312215989675E-62 ) ) ;
#766 = LINE ( 'NONE', #17049, #8494 ) ;
#767 = ORIENTED_EDGE ( 'NONE', *, *, #1383, .F. ) ;
#769 = CIRCLE ( 'NONE', #12189, 2.999765877365279998 ) ;
#768 = LINE ( 'NONE', #15389, #14688 ) ;
#770 = ADVANCED_FACE ( 'NONE', ( #18377, #4353 ), #408, .T. ) ;
#771 = DIRECTION ( 'NONE',  ( -0.9730401042858024541, 0.2306359803922080898, 5.959266323858942451E-17 ) ) ;
#772 = ORIENTED_EDGE ( 'NONE', *, *, #11755, .F. ) ;
#773 = CARTESIAN_POINT ( 'NONE',  ( 34.98595693676443830, 7.794708766260042943, -8.759424124906628251 ) ) ;
#774 = DIRECTION ( 'NONE',  ( 4.847794496894149712E-12, 0.000000000000000000, 1.000000000000000000 ) ) ;
#775 = CC_DESIGN_DATE_AND_TIME_ASSIGNMENT ( #18286, #7473, ( #9089 ) ) ;
#776 = LOCAL_TIME ( 14, 11, 27.00000000000000000, #4983 ) ;
#777 = SECURITY_CLASSIFICATION_LEVEL ( 'unclassified' ) ;
#778 = APPROVAL ( #2531, 'UNSPECIFIED' ) ;
#779 = CARTESIAN_POINT ( 'NONE',  ( 36.17078849317573486, 12.20740994216804154, 26.29999999999999005 ) ) ;
#780 = APPROVAL_PERSON_ORGANIZATION ( #7972, #9994, #9518 ) ;
#781 = ORIENTED_EDGE ( 'NONE', *, *, #11287, .F. ) ;
#782 = EDGE_CURVE ( 'NONE', #8934, #14619, #17447, .T. ) ;
#783 = EDGE_CURVE ( 'NONE', #5737, #19582, #7671, .T. ) ;
#784 = DATE_AND_TIME ( #11642, #2321 ) ;
#785 = CARTESIAN_POINT ( 'NONE',  ( 26.57755037370655060, -6.586732293730130472, -18.00000000000000000 ) ) ;
#786 = AXIS2_PLACEMENT_3D ( 'NONE', #9245, #80, #5547 ) ;
#787 = ORIENTED_EDGE ( 'NONE', *, *, #5363, .F. ) ;
#788 = ORIENTED_EDGE ( 'NONE', *, *, #11343, .T. ) ;
#789 = APPROVAL_PERSON_ORGANIZATION ( #9849, #15157, #11648 ) ;
#790 = DATE_AND_TIME ( #15295, #16404 ) ;
#791 = AXIS2_PLACEMENT_3D ( 'NONE', #18120, #19903, #8979 ) ;
#792 = EDGE_CURVE ( 'NONE', #13752, #6915, #20618, .T. ) ;
#793 = SECURITY_CLASSIFICATION_LEVEL ( 'unclassified' ) ;
#794 = DIRECTION ( 'NONE',  ( 1.426882515614939919E-15, 5.761552236122200693E-15, 1.000000000000000000 ) ) ;
#795 = PRODUCT_DEFINITION_FORMATION_WITH_SPECIFIED_SOURCE ( 'ANY', '', #3402, .NOT_KNOWN. ) ;
#796 = PRODUCT_DEFINITION_FORMATION_WITH_SPECIFIED_SOURCE ( 'ANY', '', #1104, .NOT_KNOWN. ) ;
#797 = LINE ( 'NONE', #15303, #11528 ) ;
#798 = AXIS2_PLACEMENT_3D ( 'NONE', #9639, #22071, #14833 ) ;
#799 = EDGE_LOOP ( 'NONE', ( #7526, #13181 ) ) ;
#800 = COORDINATED_UNIVERSAL_TIME_OFFSET ( 0, 0, .AHEAD. ) ;
#801 = EDGE_CURVE ( 'NONE', #547, #8431, #4543, .T. ) ;
#802 = ORIENTED_EDGE ( 'NONE', *, *, #16504, .F. ) ;
#803 = APPROVAL_PERSON_ORGANIZATION ( #16233, #14580, #19796 ) ;
#804 = CYLINDRICAL_SURFACE ( 'NONE', #4227, 4.250000000000000000 ) ;
#805 = DIRECTION ( 'NONE',  ( 0.000000000000000000, -1.000000000000000000, 0.000000000000000000 ) ) ;
#806 = ORIENTED_EDGE ( 'NONE', *, *, #4181, .T. ) ;
#807 = CC_DESIGN_PERSON_AND_ORGANIZATION_ASSIGNMENT ( #13789, #21132, ( #10100 ) ) ;
#808 = CARTESIAN_POINT ( 'NONE',  ( -62.74088165156670271, -25.10566213532069924, -5.538319619822460249E-15 ) ) ;
#809 = CC_DESIGN_PERSON_AND_ORGANIZATION_ASSIGNMENT ( #8697, #5009, ( #7614 ) ) ;
#810 = FACE_OUTER_BOUND ( 'NONE', #9895, .T. ) ;
#811 = FACE_OUTER_BOUND ( 'NONE', #5010, .T. ) ;
#812 = EDGE_LOOP ( 'NONE', ( #1100, #19503 ) ) ;
#813 = VERTEX_POINT ( 'NONE', #7558 ) ;
#814 = CARTESIAN_POINT ( 'NONE',  ( 35.59419854219520118, 9.774809681453319854, -20.00000000000000000 ) ) ;
#815 = VERTEX_POINT ( 'NONE', #14791 ) ;
#816 = EDGE_CURVE ( 'NONE', #8039, #560, #11774, .T. ) ;
#817 = EDGE_CURVE ( 'NONE', #7141, #2857, #17822, .T. ) ;
#818 = DATE_AND_TIME ( #13434, #17498 ) ;
#819 = CC_DESIGN_APPROVAL ( #6025, ( #15633 ) ) ;
#820 = EDGE_LOOP ( 'NONE', ( #21384, #19858, #16833, #7927, #3627, #11636, #14084, #7098, #6887, #15761, #3055 ) ) ;
#821 = ORIENTED_EDGE ( 'NONE', *, *, #18406, .T. ) ;
#822 = DIRECTION ( 'NONE',  ( -0.9730401042858036753, 0.2306359803922031493, -2.740969466505752002E-16 ) ) ;
#823 = DATE_AND_TIME ( #16987, #15241 ) ;
#824 = AXIS2_PLACEMENT_3D ( 'NONE', #5294, #21212, #10795 ) ;
#825 = CARTESIAN_POINT ( 'NONE',  ( -16.50000000000000000, -20.00000000000000000, -2.500000000000000000 ) ) ;
#826 = AXIS2_PLACEMENT_3D ( 'NONE', #11250, #2075, #14665 ) ;
#827 = ORGANIZATION ( 'NAUO-ORG36', 'UNSPECIFIED', 'UNSPECIFIED' ) ;
#828 = VECTOR ( 'NONE', #6564, 1000.000000000000227 ) ;
#829 = AXIS2_PLACEMENT_3D ( 'NONE', #12501, #11670, #16865 ) ;
#830 = CARTESIAN_POINT ( 'NONE',  ( 0.000000000000000000, 0.000000000000000000, 0.000000000000000000 ) ) ;
#831 = DIRECTION ( 'NONE',  ( 9.248903203239929993E-11, -1.000000000000000000, 2.220446028257650359E-15 ) ) ;
#832 = CALENDAR_DATE ( 2026, 31, 10 ) ;
#833 = EDGE_CURVE ( 'NONE', #21153, #11037, #11400, .T. ) ;
#834 = LOCAL_TIME ( 14, 11, 27.00000000000000000, #21216 ) ;
#835 = EDGE_LOOP ( 'NONE', ( #18572, #6387, #5967, #11547 ) ) ;
#836 = CARTESIAN_POINT ( 'NONE',  ( 34.43023877205762062, 1.829043660892520684, 13.00000000000000000 ) ) ;
#837 = AXIS2_PLACEMENT_3D ( 'NONE', #5349, #16154, #3336 ) ;
#838 = ORIENTED_EDGE ( 'NONE', *, *, #7929, .T. ) ;
#839 = VECTOR ( 'NONE', #16919, 1000.000000000000000 ) ;
#840 = ADVANCED_FACE ( 'NONE', ( #2911 ), #9485, .F. ) ;
#841 = CARTESIAN_POINT ( 'NONE',  ( -26.99999999999959854, -31.09999999999999787, -22.00000000000000000 ) ) ;
#842 = VECTOR ( 'NONE', #12317, 1000.000000000000000 ) ;
#843 = CARTESIAN_POINT ( 'NONE',  ( -25.49858938551139786, -0.2322002804899490069, -5.000000000000000000 ) ) ;
#844 = ORIENTED_EDGE ( 'NONE', *, *, #5443, .T. ) ;
#845 = DIRECTION ( 'NONE',  ( 1.138590270679734009E-14, 2.220446049251240387E-15, 1.000000000000000000 ) ) ;
#846 = ADVANCED_FACE ( 'NONE', ( #11729 ), #15615, .T. ) ;
#847 = AXIS2_PLACEMENT_3D ( 'NONE', #20575, #20337, #11694 ) ;
#848 = COORDINATED_UNIVERSAL_TIME_OFFSET ( 0, 0, .AHEAD. ) ;
#850 = EDGE_CURVE ( 'NONE', #8336, #4807, #22966, .T. ) ;
#849 = EDGE_LOOP ( 'NONE', ( #17166, #16409 ) ) ;
#851 = VERTEX_POINT ( 'NONE', #22856 ) ;
#852 = DIRECTION ( 'NONE',  ( 3.210834492194349687E-17, -2.441916418604790135E-15, -1.000000000000000000 ) ) ;
#853 = CARTESIAN_POINT ( 'NONE',  ( -20.00000000000000000, -20.00000000000000000, 5.000000000004559908 ) ) ;
#854 = VECTOR ( 'NONE', #2228, 999.9999999999998863 ) ;
#855 = FACE_BOUND ( 'NONE', #20769, .T. ) ;
#856 = APPROVAL_STATUS ( 'not_yet_approved' ) ;
#857 = CONICAL_SURFACE ( 'NONE', #20602, 2.624999999999998668, 0.4636476090008128104 ) ;
#858 = CARTESIAN_POINT ( 'NONE',  ( 122.7747609327790030, 11.20643158045800014, -9.133960000000000079 ) ) ;
#859 = LOCAL_TIME ( 14, 11, 27.00000000000000000, #8381 ) ;
#860 = LINE ( 'NONE', #8129, #5700 ) ;
#861 = CONTEXT_DEPENDENT_SHAPE_REPRESENTATION ( #7195, #964 ) ;
#862 = AXIS2_PLACEMENT_3D ( 'NONE', #21364, #5207, #8777 ) ;
#863 = CARTESIAN_POINT ( 'NONE',  ( -25.65326162860803194, 22.49081825942809942, 2.499999999999996891 ) ) ;
#864 = CIRCLE ( 'NONE', #13389, 2.500000000000000444 ) ;
#865 = ADVANCED_BREP_SHAPE_REPRESENTATION ( '', ( #17019, #12739 ), #15936 ) ;
#866 = VECTOR ( 'NONE', #10324, 1000.000000000000000 ) ;
#867 = DIRECTION ( 'NONE',  ( 0.2306359803922095053, 0.9730401042858018990, 0.000000000000000000 ) ) ;
#868 = APPROVAL_DATE_TIME ( #1331, #12792 ) ;
#869 = DIRECTION ( 'NONE',  ( -3.469446951953612296E-14, -1.908195823574486794E-13, -1.000000000000000000 ) ) ;
#870 = AXIS2_PLACEMENT_3D ( 'NONE', #14772, #9688, #624 ) ;
#871 = DIRECTION ( 'NONE',  ( -0.6880432561069586006, 0.1630842657209347069, -0.7071067811865459074 ) ) ;
#872 = AXIS2_PLACEMENT_3D ( 'NONE', #8546, #19572, #23111 ) ;
#873 = CC_DESIGN_PERSON_AND_ORGANIZATION_ASSIGNMENT ( #15362, #11822, ( #12089 ) ) ;
#874 = PLANE ( 'NONE',  #17305 ) ;
#875 = LOCAL_TIME ( 14, 11, 27.00000000000000000, #15000 ) ;
#876 = CARTESIAN_POINT ( 'NONE',  ( 33.72726576586480007, 23.57751093912980167, -13.00000000000030020 ) ) ;
#877 = PLANE ( 'NONE',  #20182 ) ;
#878 = AXIS2_PLACEMENT_3D ( 'NONE', #4658, #15014, #6561 ) ;
#879 = DIRECTION ( 'NONE',  ( 0.1997366180463766849, 0.8426774492125652660, -0.5000000000000004441 ) ) ;
#880 = AXIS2_PLACEMENT_3D ( 'NONE', #3587, #2349, #21614 ) ;
#881 = ORIENTED_EDGE ( 'NONE', *, *, #15797, .T. ) ;
#882 = AXIS2_PLACEMENT_3D ( 'NONE', #3490, #23429, #9309 ) ;
#883 = ORIENTED_EDGE ( 'NONE', *, *, #14280, .F. ) ;
#884 = DIRECTION ( 'NONE',  ( 0.2306359803922053697, 0.9730401042858028982, 0.000000000000000000 ) ) ;
#885 = DIRECTION ( 'NONE',  ( -1.578894428126670167E-37, -2.578073951805180219E-21, 1.000000000000000000 ) ) ;
#886 = VERTEX_POINT ( 'NONE', #6361 ) ;
#887 = CARTESIAN_POINT ( 'NONE',  ( -19.99975861755300244, 22.95209442650120124, 4.999999999999900524 ) ) ;
#888 = ORIENTED_EDGE ( 'NONE', *, *, #14022, .T. ) ;
#889 = CARTESIAN_POINT ( 'NONE',  ( 102.8131131701580046, 7.202356331284519797, 13.00000000000000000 ) ) ;
#890 = COORDINATED_UNIVERSAL_TIME_OFFSET ( 0, 0, .AHEAD. ) ;
#891 = LINE ( 'NONE', #1118, #14675 ) ;
#892 = EDGE_CURVE ( 'NONE', #2209, #19953, #2563, .T. ) ;
#893 = AXIS2_PLACEMENT_3D ( 'NONE', #20849, #2461, #4233 ) ;
#894 = DATE_TIME_ROLE ( 'classification_date' ) ;
#895 =( LENGTH_UNIT ( ) NAMED_UNIT ( * ) SI_UNIT ( .MILLI., .METRE. ) );
#896 = VECTOR ( 'NONE', #18174, 1000.000000000000000 ) ;
#897 = CARTESIAN_POINT ( 'NONE',  ( -0.1773429184338829179, 15.53017835561892213, -7.303449571161556722E-15 ) ) ;
#898 = FACE_OUTER_BOUND ( 'NONE', #11137, .T. ) ;
#899 = FACE_OUTER_BOUND ( 'NONE', #15070, .T. ) ;
#900 = ORIENTED_EDGE ( 'NONE', *, *, #21861, .T. ) ;
#901 = LINE ( 'NONE', #4002, #22309 ) ;
#902 = CARTESIAN_POINT ( 'NONE',  ( 111.8137341348020044, 5.068973512656540059, -13.00000000000000000 ) ) ;
#903 = VERTEX_POINT ( 'NONE', #10178 ) ;
#904 = DIRECTION ( 'NONE',  ( 0.9730401042858035643, -0.2306359803922028717, 2.740969466505749044E-16 ) ) ;
#905 = DIRECTION ( 'NONE',  ( 1.138590270679728013E-14, 2.220446049251240387E-15, 1.000000000000000000 ) ) ;
#906 = CONICAL_SURFACE ( 'NONE', #14198, 1.154700538379250796, 1.047197551196598297 ) ;
#907 = DATE_AND_TIME ( #13742, #13747 ) ;
#908 = DIRECTION ( 'NONE',  ( -0.9730401042858035643, 0.2306359803922028717, 5.432877459303547053E-17 ) ) ;
#909 =( BOUNDED_CURVE ( )  B_SPLINE_CURVE ( 2, ( #15250, #2658, #18475 ),
 .UNSPECIFIED., .F., .F. ) 
 B_SPLINE_CURVE_WITH_KNOTS ( ( 3, 3 ),
 ( 0.000000000000000000, 0.5842180690389598974 ),
 .UNSPECIFIED. ) 
 CURVE ( )  GEOMETRIC_REPRESENTATION_ITEM ( )  RATIONAL_B_SPLINE_CURVE ( ( 1.000000000000000000, 1.154700538379259900, 1.000000000000000000 ) ) 
 REPRESENTATION_ITEM ( '' )  );
#910 = ORIENTED_EDGE ( 'NONE', *, *, #17387, .F. ) ;
#911 = VECTOR ( 'NONE', #21579, 1000.000000000000227 ) ;
#912 = ORIENTED_EDGE ( 'NONE', *, *, #11481, .F. ) ;
#913 = COORDINATED_UNIVERSAL_TIME_OFFSET ( 0, 0, .AHEAD. ) ;
#914 = CYLINDRICAL_SURFACE ( 'NONE', #8817, 3.500000000000000444 ) ;
#915 = ORIENTED_EDGE ( 'NONE', *, *, #10858, .F. ) ;
#916 = ORIENTED_EDGE ( 'NONE', *, *, #3595, .T. ) ;
#917 = FACE_OUTER_BOUND ( 'NONE', #4736, .T. ) ;
#918 = CALENDAR_DATE ( 2026, 31, 10 ) ;
#919 = EDGE_CURVE ( 'NONE', #8630, #18569, #15543, .T. ) ;
#920 = CARTESIAN_POINT ( 'NONE',  ( -26.68810977484059777, -6.639828994528089723, -2.501000000000090484 ) ) ;
#921 = APPROVAL ( #8049, 'UNKNOWN' ) ;
#922 = CYLINDRICAL_SURFACE ( 'NONE', #4671, 5.999999999999999112 ) ;
#923 = ORIENTED_EDGE ( 'NONE', *, *, #4260, .T. ) ;
#924 = APPLICATION_CONTEXT ( 'configuration controlled 3d designs of mechanical parts and assemblies' ) ;
#925 = ADVANCED_FACE ( 'NONE', ( #755, #13953 ), #20960, .T. ) ;
#926 = ADVANCED_FACE ( 'NONE', ( #995 ), #22736, .F. ) ;
#927 = CALENDAR_DATE ( 2026, 31, 10 ) ;
#928 = VERTEX_POINT ( 'NONE', #15265 ) ;
#929 = DIRECTION ( 'NONE',  ( -4.028143194477080210E-16, -2.054129435991050111E-15, -1.000000000000000000 ) ) ;
#930 = DIRECTION ( 'NONE',  ( 0.2306359803922031215, 0.9730401042858035643, -1.407521210652540770E-17 ) ) ;
#931 = ORIENTED_EDGE ( 'NONE', *, *, #4009, .T. ) ;
#932 = DIRECTION ( 'NONE',  ( -0.02168293104353429326, 0.9997648976141146893, -2.442038521257509372E-15 ) ) ;
#933 = DIRECTION ( 'NONE',  ( 0.7071067811865476838, -1.387778780781444689E-15, 0.7071067811865473507 ) ) ;
#934 = DIRECTION ( 'NONE',  ( 0.000000000000000000, 1.020425574104004122E-16, 1.000000000000000000 ) ) ;
#935 = VERTEX_POINT ( 'NONE', #4701 ) ;
#936 = ORIENTED_EDGE ( 'NONE', *, *, #1650, .T. ) ;
#937 = CARTESIAN_POINT ( 'NONE',  ( 55.46237324781409939, -8.294657213477510282, -13.00000000000000000 ) ) ;
#938 = EDGE_LOOP ( 'NONE', ( #15699, #5790, #23257, #12732, #11651 ) ) ;
#939 = APPROVAL_STATUS ( 'not_yet_approved' ) ;
#940 = ORIENTED_EDGE ( 'NONE', *, *, #10661, .T. ) ;
#941 = VECTOR ( 'NONE', #794, 1000.000000000000000 ) ;
#942 = ORIENTED_EDGE ( 'NONE', *, *, #11617, .F. ) ;
#943 = LINE ( 'NONE', #13788, #20944 ) ;
#944 = APPLICATION_PROTOCOL_DEFINITION ( 'international standard', 'config_control_design', 1994, #9637 ) ;
#945 = EDGE_CURVE ( 'NONE', #10921, #668, #8380, .T. ) ;
#946 = PLANE ( 'NONE',  #6699 ) ;
#947 = APPROVAL ( #23460, 'UNSPECIFIED' ) ;
#948 = CC_DESIGN_DATE_AND_TIME_ASSIGNMENT ( #22051, #7816, ( #19247 ) ) ;
#949 = ADVANCED_FACE ( 'NONE', ( #6248 ), #2674, .F. ) ;
#950 = EDGE_CURVE ( 'NONE', #15424, #21777, #11621, .T. ) ;
#951 = DIRECTION ( 'NONE',  ( 0.000000000000000000, -6.936119456125000933E-16, 1.000000000000000000 ) ) ;
#952 = CALENDAR_DATE ( 2026, 31, 10 ) ;
#953 = AXIS2_PLACEMENT_3D ( 'NONE', #11024, #12350, #3295 ) ;
#954 = CC_DESIGN_PERSON_AND_ORGANIZATION_ASSIGNMENT ( #19379, #8584, ( #21633 ) ) ;
#955 = EDGE_LOOP ( 'NONE', ( #3394, #13500, #9545, #120 ) ) ;
#956 = CARTESIAN_POINT ( 'NONE',  ( 58.25686728443101003, 17.76335315678745630, -10.50000000000049916 ) ) ;
#957 = LINE ( 'NONE', #10246, #10551 ) ;
#958 = ORIENTED_EDGE ( 'NONE', *, *, #5201, .T. ) ;
#959 = CARTESIAN_POINT ( 'NONE',  ( 0.000000000000000000, 0.000000000000000000, -5.000000000000000000 ) ) ;
#960 = LINE ( 'NONE', #12148, #70 ) ;
#961 = ORIENTED_EDGE ( 'NONE', *, *, #1763, .T. ) ;
#962 = DIRECTION ( 'NONE',  ( -0.9997651245102161521, -0.02167246670483386276, 0.000000000000000000 ) ) ;
#963 = PERSON_AND_ORGANIZATION_ROLE ( 'classification_officer' ) ;
#964 = PRODUCT_DEFINITION_SHAPE ( 'NONE', 'NONE',  #23480 ) ;
#965 = VERTEX_POINT ( 'NONE', #17524 ) ;
#966 = ORIENTED_EDGE ( 'NONE', *, *, #9719, .T. ) ;
#967 = LINE ( 'NONE', #14035, #9624 ) ;
#968 = CARTESIAN_POINT ( 'NONE',  ( 31.37708959083939675, -0.2124270449898580104, -13.00000000000039968 ) ) ;
#969 = ORIENTED_EDGE ( 'NONE', *, *, #9231, .F. ) ;
#970 = CALENDAR_DATE ( 2026, 31, 10 ) ;
#971 = LINE ( 'NONE', #4195, #1255 ) ;
#972 = ADVANCED_FACE ( 'NONE', ( #1236 ), #9940, .T. ) ;
#973 = CARTESIAN_POINT ( 'NONE',  ( 37.88245768368250310, -4.127756955731490152, -13.00000000000000000 ) ) ;
#974 = DIRECTION ( 'NONE',  ( -0.9999862922474492821, -0.005235963827121953122, 1.466966272682004590E-16 ) ) ;
#975 = AXIS2_PLACEMENT_3D ( 'NONE', #21938, #1876, #5674 ) ;
#976 = ADVANCED_FACE ( 'NONE', ( #20840 ), #17168, .F. ) ;
#977 = EDGE_CURVE ( 'NONE', #20686, #18898, #22608, .T. ) ;
#978 = CARTESIAN_POINT ( 'NONE',  ( -27.00000000000000000, -28.60000000000000142, -19.00000000000000000 ) ) ;
#979 = PERSON_AND_ORGANIZATION ( #11966, #8758 ) ;
#980 = EDGE_CURVE ( 'NONE', #677, #22280, #5671, .T. ) ;
#981 = CARTESIAN_POINT ( 'NONE',  ( 35.59419854219520118, 9.774809681453540122, 26.50000000000000000 ) ) ;
#982 = FACE_OUTER_BOUND ( 'NONE', #5351, .T. ) ;
#983 = CARTESIAN_POINT ( 'NONE',  ( 114.9904400984929254, 13.05151942359561978, 2.500000000000071498 ) ) ;
#984 = VECTOR ( 'NONE', #14388, 1000.000000000000227 ) ;
#985 = PLANE ( 'NONE',  #9370 ) ;
#986 = VECTOR ( 'NONE', #16074, 1000.000000000000000 ) ;
#987 = DIRECTION ( 'NONE',  ( 3.099353312215988811E-62, -1.534091707905539548E-92, -1.000000000000000000 ) ) ;
#988 = DIRECTION ( 'NONE',  ( -3.099353312215988811E-62, -9.818186930595456717E-93, 1.000000000000000000 ) ) ;
#989 = VERTEX_POINT ( 'NONE', #6967 ) ;
#990 = VERTEX_POINT ( 'NONE', #3152 ) ;
#991 = DIRECTION ( 'NONE',  ( -0.1153179901961009640, -0.4865200521429018377, -0.8660254037844385966 ) ) ;
#992 = ORIENTED_EDGE ( 'NONE', *, *, #14588, .T. ) ;
#993 = DIRECTION ( 'NONE',  ( -0.2306359803922033158, -0.9730401042858034533, 0.000000000000000000 ) ) ;
#994 = ORIENTED_EDGE ( 'NONE', *, *, #10741, .F. ) ;
#995 = FACE_OUTER_BOUND ( 'NONE', #9985, .T. ) ;
#996 = PERSON_AND_ORGANIZATION_ROLE ( 'design_supplier' ) ;
#997 = DIRECTION ( 'NONE',  ( -0.2306359803922085339, -0.9730401042858022320, 0.000000000000000000 ) ) ;
#998 = VECTOR ( 'NONE', #17041, 1000.000000000000000 ) ;
#999 = VECTOR ( 'NONE', #4794, 1000.000000000000227 ) ;
#1000 = CIRCLE ( 'NONE', #12790, 0.4000000000000010214 ) ;
#1001 = ADVANCED_FACE ( 'NONE', ( #1708 ), #29, .T. ) ;
#1002 = DIRECTION ( 'NONE',  ( 2.269747459788994803E-13, 2.220446049250330436E-15, 1.000000000000000000 ) ) ;
#1003 = DIRECTION ( 'NONE',  ( -3.099353312215988811E-62, 2.485476484129594803E-78, 1.000000000000000000 ) ) ;
#1004 = DIRECTION ( 'NONE',  ( 0.000000000000000000, 0.000000000000000000, -1.000000000000000000 ) ) ;
#1005 = VERTEX_POINT ( 'NONE', #17999 ) ;
#1006 = CARTESIAN_POINT ( 'NONE',  ( 122.4288069621910040, 9.746871424029270869, 10.02499999999999858 ) ) ;
#1007 = LINE ( 'NONE', #16940, #9510 ) ;
#1008 = VERTEX_POINT ( 'NONE', #8728 ) ;
#1009 = AXIS2_PLACEMENT_3D ( 'NONE', #11223, #5852, #364 ) ;
#1010 = DIRECTION ( 'NONE',  ( 0.000000000000000000, 0.000000000000000000, 1.000000000000000000 ) ) ;
#1011 = LINE ( 'NONE', #15045, #7252 ) ;
#1012 = ADVANCED_FACE ( 'NONE', ( #7078 ), #21648, .T. ) ;
#1013 = AXIS2_PLACEMENT_3D ( 'NONE', #2652, #17386, #9912 ) ;
#1014 = PERSON_AND_ORGANIZATION ( #11923, #22834 ) ;
#1015 = DIRECTION ( 'NONE',  ( -0.005235963827121951387, 0.9999862922474492821, 7.400535959139851804E-19 ) ) ;
#1016 = AXIS2_PLACEMENT_3D ( 'NONE', #4998, #12267, #10483 ) ;
#1017 = VERTEX_POINT ( 'NONE', #18105 ) ;
#1018 = ORIENTED_EDGE ( 'NONE', *, *, #18119, .T. ) ;
#1019 = PERSON_AND_ORGANIZATION ( #11966, #8758 ) ;
#1020 = CARTESIAN_POINT ( 'NONE',  ( 33.27705887009660302, -3.036156860536630031, -13.00000000000000000 ) ) ;
#1021 = ORIENTED_EDGE ( 'NONE', *, *, #17513, .F. ) ;
#1022 = CARTESIAN_POINT ( 'NONE',  ( 34.94102482032229773, 25.66320561742219653, 13.00000000000000000 ) ) ;
#1023 = CIRCLE ( 'NONE', #4074, 6.500000000000000000 ) ;
#1024 = DATE_TIME_ROLE ( 'creation_date' ) ;
#1025 = DATE_AND_TIME ( #8542, #14470 ) ;
#1026 = VECTOR ( 'NONE', #20309, 1000.000000000000227 ) ;
#1027 = DIRECTION ( 'NONE',  ( 0.000000000000000000, -2.739767185169287006E-14, 1.000000000000000000 ) ) ;
#1028 = AXIS2_PLACEMENT_3D ( 'NONE', #21199, #4821, #19313 ) ;
#1029 = CIRCLE ( 'NONE', #16222, 6.499999999999997335 ) ;
#1030 = CONICAL_SURFACE ( 'NONE', #14324, 2.283500000000000085, 0.7853981633974469467 ) ;
#1031 = CYLINDRICAL_SURFACE ( 'NONE', #10387, 4.250000000000001776 ) ;
#1032 = ORIENTED_EDGE ( 'NONE', *, *, #1810, .T. ) ;
#1033 = APPROVAL_ROLE ( '' ) ;
#1034 = EDGE_LOOP ( 'NONE', ( #6117, #22983, #18814, #12355 ) ) ;
#1035 = CIRCLE ( 'NONE', #10560, 2.500000000000000000 ) ;
#1036 = CARTESIAN_POINT ( 'NONE',  ( 35.07420204808332898, 7.580974001528502093, -10.74538000000048932 ) ) ;
#1037 = CARTESIAN_POINT ( 'NONE',  ( 37.27955344062029752, 9.375336445360519022, -27.69000000000049866 ) ) ;
#1039 = ORIENTED_EDGE ( 'NONE', *, *, #16207, .T. ) ;
#1038 = EDGE_CURVE ( 'NONE', #14262, #8503, #5056, .T. ) ;
#1040 = EDGE_CURVE ( 'NONE', #22846, #5938, #22362, .T. ) ;
#1041 = FACE_OUTER_BOUND ( 'NONE', #16334, .T. ) ;
#1042 = DIRECTION ( 'NONE',  ( 0.9999862922474493931, 0.005235963827108368503, 0.000000000000000000 ) ) ;
#1043 = CARTESIAN_POINT ( 'NONE',  ( 35.35837847849400362, 22.00420084508149898, -11.00000000000049916 ) ) ;
#1044 = VECTOR ( 'NONE', #14926, 1000.000000000000114 ) ;
#1045 = ORIENTED_EDGE ( 'NONE', *, *, #7237, .F. ) ;
#1046 = ORIENTED_EDGE ( 'NONE', *, *, #17043, .T. ) ;
#1047 = DIRECTION ( 'NONE',  ( 2.528178268246854219E-29, 2.220446049251370154E-15, 1.000000000000000000 ) ) ;
#1048 = ORIENTED_EDGE ( 'NONE', *, *, #465, .F. ) ;
#1049 = APPROVAL_ROLE ( '' ) ;
#1050 = CONICAL_SURFACE ( 'NONE', #16592, 2.283500000000000085, 0.7853981633974469467 ) ;
#1051 = ORIENTED_EDGE ( 'NONE', *, *, #20948, .T. ) ;
#1052 = EDGE_LOOP ( 'NONE', ( #5105, #5858, #452, #9952 ) ) ;
#1053 = DIRECTION ( 'NONE',  ( -0.9997648975362233292, -0.02168293463497958373, 0.000000000000000000 ) ) ;
#1054 = AXIS2_PLACEMENT_3D ( 'NONE', #7400, #18558, #13322 ) ;
#1055 = APPROVAL_DATE_TIME ( #22916, #19129 ) ;
#1056 = ADVANCED_FACE ( 'NONE', ( #12193 ), #10419, .T. ) ;
#1057 = EDGE_CURVE ( 'NONE', #9718, #13613, #21310, .T. ) ;
#1058 = DIRECTION ( 'NONE',  ( -0.9999862922474492821, -0.005235963827121951387, 1.466966272682004590E-16 ) ) ;
#1059 = PLANE ( 'NONE',  #3913 ) ;
#1060 = CARTESIAN_POINT ( 'NONE',  ( 36.09092202081949807, 8.115512906978191054, -28.47000000000049980 ) ) ;
#1061 = APPROVAL_DATE_TIME ( #4761, #4793 ) ;
#1062 = VECTOR ( 'NONE', #21138, 1000.000000000000000 ) ;
#1063 = VERTEX_POINT ( 'NONE', #17759 ) ;
#1064 = CARTESIAN_POINT ( 'NONE',  ( -17.47493719149670000, 26.45208920939580111, 6.750000000004429346 ) ) ;
#1065 = CARTESIAN_POINT ( 'NONE',  ( 35.59419854219520118, 9.774809681453469068, 10.50000000000020073 ) ) ;
#1066 = ORIENTED_EDGE ( 'NONE', *, *, #2450, .T. ) ;
#1067 = EDGE_CURVE ( 'NONE', #11527, #12850, #6836, .T. ) ;
#1068 = CARTESIAN_POINT ( 'NONE',  ( 112.6956120935900003, 3.369770385951889935, 3.165715546043859906E-14 ) ) ;
#1069 = CARTESIAN_POINT ( 'NONE',  ( -29.94686441333699989, 7.343408934390589948, 5.000000000000000000 ) ) ;
#1070 = CARTESIAN_POINT ( 'NONE',  ( 43.14167273007649328, 18.99928136731766770, 13.00000000000000000 ) ) ;
#1071 = ORIENTED_EDGE ( 'NONE', *, *, #16968, .T. ) ;
#1072 = DIRECTION ( 'NONE',  ( -0.9730401042858024541, 0.2306359803922080898, 5.959266323853792669E-17 ) ) ;
#1073 = CC_DESIGN_PERSON_AND_ORGANIZATION_ASSIGNMENT ( #12818, #5675, ( #7962 ) ) ;
#1074 = MECHANICAL_CONTEXT ( 'NONE', #3800, 'mechanical' ) ;
#1075 = ORIENTED_EDGE ( 'NONE', *, *, #11246, .F. ) ;
#1076 = CC_DESIGN_PERSON_AND_ORGANIZATION_ASSIGNMENT ( #6694, #8704, ( #19920 ) ) ;
#1077 = EDGE_LOOP ( 'NONE', ( #8086, #17726, #7326, #4054 ) ) ;
#1078 = CARTESIAN_POINT ( 'NONE',  ( 53.10252809683450437, 27.27557781334509812, 3.299332471243299474E-14 ) ) ;
#1079 = DIRECTION ( 'NONE',  ( -0.2306359803922033713, -0.9730401042858034533, 4.558064749665356219E-15 ) ) ;
#1080 = ORIENTED_EDGE ( 'NONE', *, *, #8568, .T. ) ;
#1081 = APPROVAL_DATE_TIME ( #3465, #3566 ) ;
#1082 = ADVANCED_FACE ( 'NONE', ( #15852 ), #3259, .F. ) ;
#1083 = CARTESIAN_POINT ( 'NONE',  ( 113.9197686726213448, -24.27486053345101169, 13.00000000000000000 ) ) ;
#1084 = EDGE_CURVE ( 'NONE', #544, #15192, #15963, .T. ) ;
#1085 = CLOSED_SHELL ( 'NONE', ( #12715, #9280, #8950, #16235, #5596, #17857, #8299, #2010, #10563, #625, #19739, #11686, #14339, #12107, #384, #18950, #16345, #13405, #7191, #12169, #14207, #10751, #7480, #19339, #20276 ) ) ;
#1086 = DIRECTION ( 'NONE',  ( 0.005235963827101452160, -0.9999862922474493931, 5.479105319409471602E-16 ) ) ;
#1087 = PERSON_AND_ORGANIZATION_ROLE ( 'classification_officer' ) ;
#1088 = ADVANCED_FACE ( 'NONE', ( #16198 ), #12427, .F. ) ;
#1089 = DIRECTION ( 'NONE',  ( -0.005235963827121941846, 0.9999862922474492821, 5.936218956651588485E-19 ) ) ;
#1090 =( NAMED_UNIT ( * ) PLANE_ANGLE_UNIT ( ) SI_UNIT ( $, .RADIAN. ) );
#1091 = CIRCLE ( 'NONE', #7186, 4.750000000000001776 ) ;
#1092 = DIRECTION ( 'NONE',  ( -1.000000000000000000, -6.662112528310618598E-09, 2.269018306577664942E-13 ) ) ;
#1093 = PERSON_AND_ORGANIZATION_ROLE ( 'design_owner' ) ;
#1094 = CARTESIAN_POINT ( 'NONE',  ( 36.69650084708651150, 11.52859305909626286, 8.783982963266916855 ) ) ;
#1095 = CARTESIAN_POINT ( 'NONE',  ( 5.000000000000000000, -28.60000000000000142, -19.00000000000000000 ) ) ;
#1096 = FACE_OUTER_BOUND ( 'NONE', #15890, .T. ) ;
#1097 = EDGE_CURVE ( 'NONE', #11267, #11726, #12532, .T. ) ;
#1098 = DIRECTION ( 'NONE',  ( -0.2306359803922033436, -0.9730401042858034533, 0.000000000000000000 ) ) ;
#1099 = CARTESIAN_POINT ( 'NONE',  ( -23.50000000000000000, -20.00000000000000000, -2.500000000000000000 ) ) ;
#1100 = ORIENTED_EDGE ( 'NONE', *, *, #16646, .T. ) ;
#1101 =( REPRESENTATION_RELATIONSHIP ('NONE','NONE', #19303, #7169 ) REPRESENTATION_RELATIONSHIP_WITH_TRANSFORMATION ( #19081 )SHAPE_REPRESENTATION_RELATIONSHIP( ) );
#1102 = DIRECTION ( 'NONE',  ( 1.751019220569994795E-16, 2.300154215587015208E-15, 1.000000000000000000 ) ) ;
#1103 = ORIENTED_EDGE ( 'NONE', *, *, #9591, .F. ) ;
#1104 = PRODUCT ( '1602p_c_33', '1602p_c_33', '', ( #22706 ) ) ;
#1105 = EDGE_LOOP ( 'NONE', ( #15851, #7040, #21791, #2059 ) ) ;
#1106 = CARTESIAN_POINT ( 'NONE',  ( 122.4288069621910040, 9.746871424029281528, -13.00000000000000000 ) ) ;
#1107 = SHAPE_REPRESENTATION ( '1602p_c_42', ( #12739 ), #11790 ) ;
#1108 = CYLINDRICAL_SURFACE ( 'NONE', #17422, 6.500000000000000000 ) ;
#1109 = ORGANIZATION ( 'NAUO-ORG6', 'UNSPECIFIED', 'UNSPECIFIED' ) ;
#1110 = VERTEX_POINT ( 'NONE', #3371 ) ;
#1111 = CIRCLE ( 'NONE', #12874, 0.0009999999999975306419 ) ;
#1112 = ADVANCED_FACE ( 'NONE', ( #10642 ), #2941, .T. ) ;
#1113 = CARTESIAN_POINT ( 'NONE',  ( -27.00000000000000000, -29.85000000000000142, -12.00000000000000000 ) ) ;
#1114 = EDGE_CURVE ( 'NONE', #21559, #18063, #16209, .T. ) ;
#1115 = EDGE_LOOP ( 'NONE', ( #6960, #12459 ) ) ;
#1116 = DIRECTION ( 'NONE',  ( -3.469446951953612296E-14, -1.908195823574486794E-13, -1.000000000000000000 ) ) ;
#1117 = CALENDAR_DATE ( 2026, 31, 10 ) ;
#1118 = CARTESIAN_POINT ( 'NONE',  ( -32.64682763696299617, 7.329162855357659545, -3.750000000000000000 ) ) ;
#1119 = PERSON_AND_ORGANIZATION_ROLE ( 'classification_officer' ) ;
#1120 =( NAMED_UNIT ( * ) SI_UNIT ( $, .STERADIAN. ) SOLID_ANGLE_UNIT ( ) );
#1121 = DIRECTION ( 'NONE',  ( -3.099353312215989243E-62, 2.537976065170614732E-77, 1.000000000000000000 ) ) ;
#1122 = VECTOR ( 'NONE', #13490, 1000.000000000000114 ) ;
#1123 = PLANE ( 'NONE',  #20252 ) ;
#1124 = VECTOR ( 'NONE', #10110, 1000.000000000000000 ) ;
#1125 = ORIENTED_EDGE ( 'NONE', *, *, #8683, .F. ) ;
#1126 = DIRECTION ( 'NONE',  ( -1.000000000000000000, -6.662112528310618598E-09, 2.269018306577664942E-13 ) ) ;
#1127 = EDGE_CURVE ( 'NONE', #13630, #15927, #19891, .T. ) ;
#1128 = LINE ( 'NONE', #19662, #18640 ) ;
#1129 = ORIENTED_EDGE ( 'NONE', *, *, #17707, .F. ) ;
#1130 = CARTESIAN_POINT ( 'NONE',  ( 34.28006175981952453, 11.39274844856495683, -8.911849358505339325 ) ) ;
#1131 = DIRECTION ( 'NONE',  ( 2.528178268246854219E-29, 2.220446049251370154E-15, 1.000000000000000000 ) ) ;
#1132 = AXIS2_PLACEMENT_3D ( 'NONE', #13582, #7283, #14395 ) ;
#1133 = EDGE_CURVE ( 'NONE', #12333, #15644, #7534, .T. ) ;
#1134 = ADVANCED_FACE ( 'NONE', ( #11112, #5738 ), #16898, .T. ) ;
#1135 = DATE_AND_TIME ( #18761, #7672 ) ;
#1136 = CYLINDRICAL_SURFACE ( 'NONE', #4694, 0.4000000000000010214 ) ;
#1137 = VERTEX_POINT ( 'NONE', #21778 ) ;
#1138 = VERTEX_POINT ( 'NONE', #22231 ) ;
#1139 = EDGE_CURVE ( 'NONE', #5418, #22740, #19622, .T. ) ;
#1140 = APPROVAL_DATE_TIME ( #19323, #16473 ) ;
#1141 = DIRECTION ( 'NONE',  ( 0.1630842657209329583, 0.6880432561069529385, -0.7071067811865517916 ) ) ;
#1142 = VERTEX_POINT ( 'NONE', #5976 ) ;
#1143 = LOCAL_TIME ( 14, 11, 27.00000000000000000, #17327 ) ;
#1144 = EDGE_CURVE ( 'NONE', #6181, #10197, #4838, .T. ) ;
#1145 = DIRECTION ( 'NONE',  ( 4.028143194477080210E-16, 2.054129435991050111E-15, 1.000000000000000000 ) ) ;
#1146 =( GEOMETRIC_REPRESENTATION_CONTEXT ( 3 ) GLOBAL_UNCERTAINTY_ASSIGNED_CONTEXT ( ( #22398 ) ) GLOBAL_UNIT_ASSIGNED_CONTEXT ( ( #19948, #21719, #9375 ) ) REPRESENTATION_CONTEXT ( 'NONE', 'WORKASPACE' ) );
#1147 = COORDINATED_UNIVERSAL_TIME_OFFSET ( 0, 0, .AHEAD. ) ;
#1148 = VECTOR ( 'NONE', #3743, 1000.000000000000000 ) ;
#1149 = DIRECTION ( 'NONE',  ( -1.000000000000000000, 0.000000000000000000, 0.000000000000000000 ) ) ;
#1150 = VECTOR ( 'NONE', #12142, 1000.000000000000000 ) ;
#1151 = CARTESIAN_POINT ( 'NONE',  ( -19.99999998251385591, -22.62500000000000000, -8.249999999995454303 ) ) ;
#1152 = ORIENTED_EDGE ( 'NONE', *, *, #10914, .F. ) ;
#1153 = CC_DESIGN_APPROVAL ( #8675, ( #1527 ) ) ;
#1154 = ORIENTED_EDGE ( 'NONE', *, *, #5018, .T. ) ;
#1155 = SECURITY_CLASSIFICATION ( '', '', #6100 ) ;
#1156 = DIRECTION ( 'NONE',  ( 1.138590270679734009E-14, 2.220446049251240387E-15, 1.000000000000000000 ) ) ;
#1157 = DIRECTION ( 'NONE',  ( -1.138590270679730064E-14, -2.220446049251230526E-15, -1.000000000000000000 ) ) ;
#1158 = ORIENTED_EDGE ( 'NONE', *, *, #13143, .T. ) ;
#1159 = APPROVAL ( #21170, 'UNSPECIFIED' ) ;
#1160 = CIRCLE ( 'NONE', #4209, 2.500000000000000000 ) ;
#1161 = DIRECTION ( 'NONE',  ( 2.269747459788999852E-13, 2.220446049250325308E-15, 1.000000000000000000 ) ) ;
#1162 = SECURITY_CLASSIFICATION ( '', '', #21207 ) ;
#1163 = DIRECTION ( 'NONE',  ( -0.9730401042858035643, 0.2306359803922028717, 5.958148513035547083E-17 ) ) ;
#1164 = CARTESIAN_POINT ( 'NONE',  ( -28.45655959278310121, -6.649088660734180145, 0.7325259402522749097 ) ) ;
#1165 = EDGE_LOOP ( 'NONE', ( #3961, #781, #20696, #6323 ) ) ;
#1166 = EDGE_LOOP ( 'NONE', ( #4398, #7483, #5209, #13554 ) ) ;
#1167 = CARTESIAN_POINT ( 'NONE',  ( -68.51547434528259828, -24.91260405369630249, -2.885287058652779450E-14 ) ) ;
#1168 = ORIENTED_EDGE ( 'NONE', *, *, #12424, .T. ) ;
#1169 = AXIS2_PLACEMENT_3D ( 'NONE', #22497, #5878, #22361 ) ;
#1170 = DATE_AND_TIME ( #4864, #1175 ) ;
#1171 = VERTEX_POINT ( 'NONE', #18349 ) ;
#1172 = EDGE_LOOP ( 'NONE', ( #18340, #9582, #4866, #17239 ) ) ;
#1173 = DIRECTION ( 'NONE',  ( -0.9579954394086687142, -0.2867834340965179640, 1.451283422213139767E-15 ) ) ;
#1174 = PERSON_AND_ORGANIZATION ( #11966, #8758 ) ;
#1175 = LOCAL_TIME ( 14, 11, 27.00000000000000000, #15791 ) ;
#1176 = FACE_OUTER_BOUND ( 'NONE', #12104, .T. ) ;
#1177 = LOCAL_TIME ( 14, 11, 27.00000000000000000, #22923 ) ;
#1178 = VECTOR ( 'NONE', #2952, 1000.000000000000000 ) ;
#1179 = EDGE_CURVE ( 'NONE', #238, #12726, #5208, .T. ) ;
#1180 = CC_DESIGN_SECURITY_CLASSIFICATION ( #8018, ( #23491 ) ) ;
#1181 = LINE ( 'NONE', #8796, #9614 ) ;
#1182 = DIRECTION ( 'NONE',  ( 0.8846153846154072298, -0.4663213712685009837, 0.000000000000000000 ) ) ;
#1183 = DATE_AND_TIME ( #19253, #22794 ) ;
#1184 = VERTEX_POINT ( 'NONE', #2429 ) ;
#1185 = DIRECTION ( 'NONE',  ( 2.977235988022388482E-185, -9.605990953944227443E-124, -1.000000000000000000 ) ) ;
#1186 = CARTESIAN_POINT ( 'NONE',  ( 2.671834669462810119, 17.57827187707419725, -5.250000012366690783 ) ) ;
#1187 = ORIENTED_EDGE ( 'NONE', *, *, #12685, .T. ) ;
#1188 = LOCAL_TIME ( 14, 11, 27.00000000000000000, #913 ) ;
#1189 = DIRECTION ( 'NONE',  ( 6.123230199561429643E-17, 4.868008300101910084E-15, 1.000000000000000000 ) ) ;
#1190 = CARTESIAN_POINT ( 'NONE',  ( -3.458317987535632909, 19.03127855354509990, 7.999999999999996447 ) ) ;
#1191 = FACE_OUTER_BOUND ( 'NONE', #3998, .T. ) ;
#1192 = ORIENTED_EDGE ( 'NONE', *, *, #14770, .T. ) ;
#1193 = CARTESIAN_POINT ( 'NONE',  ( 34.88044566782586031, 28.44271146055899990, 12.99999999999979927 ) ) ;
#1194 = VECTOR ( 'NONE', #12004, 1000.000000000000000 ) ;
#1195 = DATE_AND_TIME ( #3340, #17855 ) ;
#1196 = ORIENTED_EDGE ( 'NONE', *, *, #1944, .T. ) ;
#1197 = ORIENTED_EDGE ( 'NONE', *, *, #21118, .F. ) ;
#1198 = CARTESIAN_POINT ( 'NONE',  ( 117.0319250210129951, -13.02226701625859917, 15.90000000000000036 ) ) ;
#1199 = DIRECTION ( 'NONE',  ( -0.1630842657209329027, -0.6880432561069529385, 0.7071067811865519026 ) ) ;
#1200 = SECURITY_CLASSIFICATION ( '', '', #3995 ) ;
#1201 = LINE ( 'NONE', #12734, #15743 ) ;
#1202 = APPROVAL_DATE_TIME ( #19619, #16184 ) ;
#1203 = CARTESIAN_POINT ( 'NONE',  ( 38.03772126950729415, -1.595291315507239682, -13.00000000000000000 ) ) ;
#1204 = CARTESIAN_POINT ( 'NONE',  ( 31.11077410011089839, -1.335996977273280262, -15.00000000000039968 ) ) ;
#1205 = CARTESIAN_POINT ( 'NONE',  ( 52.73786095581300515, -7.648876468381129889, 11.75000000000019895 ) ) ;
#1206 = ADVANCED_FACE ( 'NONE', ( #18463 ), #9683, .T. ) ;
#1207 = CC_DESIGN_APPROVAL ( #3566, ( #16907 ) ) ;
#1208 = VECTOR ( 'NONE', #1015, 1000.000000000000114 ) ;
#1209 = APPROVAL ( #23081, 'UNKNOWN' ) ;
#1210 = CARTESIAN_POINT ( 'NONE',  ( 33.27705887009690144, -3.036156860537079893, 13.00000000000019895 ) ) ;
#1211 = PERSON_AND_ORGANIZATION ( #11966, #8758 ) ;
#1212 = AXIS2_PLACEMENT_3D ( 'NONE', #4249, #19109, #17316 ) ;
#1213 = CIRCLE ( 'NONE', #14506, 1.000000000000000888 ) ;
#1214 = SECURITY_CLASSIFICATION ( '', '', #777 ) ;
#1215 = CARTESIAN_POINT ( 'NONE',  ( 36.91588945311071512, 11.36978919325550308, 8.806536740235856087 ) ) ;
#1216 = DIRECTION ( 'NONE',  ( 0.000000000000000000, 0.000000000000000000, 1.000000000000000000 ) ) ;
#1217 = EDGE_CURVE ( 'NONE', #2335, #2485, #7484, .T. ) ;
#1218 = EDGE_CURVE ( 'NONE', #8630, #115, #21883, .T. ) ;
#1219 = CARTESIAN_POINT ( 'NONE',  ( 52.73786095581300515, -7.648876468381259564, -14.25000000000040146 ) ) ;
#1220 = CARTESIAN_POINT ( 'NONE',  ( -62.91249983789198552, 7.670697574599230073, 2.108981951733699973E-15 ) ) ;
#1221 = DIRECTION ( 'NONE',  ( 0.000000000000000000, 0.000000000000000000, -1.000000000000000000 ) ) ;
#1222 = VERTEX_POINT ( 'NONE', #14653 ) ;
#1223 = CIRCLE ( 'NONE', #22093, 4.999999999999997335 ) ;
#1224 = CARTESIAN_POINT ( 'NONE',  ( 118.4388045014059969, -7.086722380115130449, 18.89999999999999858 ) ) ;
#1225 = ORIENTED_EDGE ( 'NONE', *, *, #8827, .T. ) ;
#1226 = CC_DESIGN_APPROVAL ( #4013, ( #1599 ) ) ;
#1227 = ORIENTED_EDGE ( 'NONE', *, *, #249, .T. ) ;
#1228 = DIRECTION ( 'NONE',  ( 0.005235963827117092427, -0.9999862922474493931, -2.636227439667000721E-16 ) ) ;
#1229 = DIRECTION ( 'NONE',  ( 0.000000000000000000, 0.000000000000000000, -1.000000000000000000 ) ) ;
#1230 = EDGE_LOOP ( 'NONE', ( #18458, #11550 ) ) ;
#1231 = AXIS2_PLACEMENT_3D ( 'NONE', #21907, #5416, #1725 ) ;
#1232 = CARTESIAN_POINT ( 'NONE',  ( -30.72441677844230057, -6.660963241697680282, -3.000000000000079936 ) ) ;
#1233 = MANIFOLD_SOLID_BREP ( 'Imported1', #6874 ) ;
#1234 = ORIENTED_EDGE ( 'NONE', *, *, #17100, .T. ) ;
#1235 = CIRCLE ( 'NONE', #5788, 2.500000000000001332 ) ;
#1236 = FACE_OUTER_BOUND ( 'NONE', #21795, .T. ) ;
#1237 = SECURITY_CLASSIFICATION_LEVEL ( 'unclassified' ) ;
#1238 = LINE ( 'NONE', #8512, #13178 ) ;
#1239 = EDGE_CURVE ( 'NONE', #5066, #2028, #1023, .T. ) ;
#1240 = APPROVAL_DATE_TIME ( #6477, #1209 ) ;
#1241 = CIRCLE ( 'NONE', #13381, 2.499999999999998668 ) ;
#1242 = PLANE ( 'NONE',  #5424 ) ;
#1243 = APPROVAL ( #11535, 'UNSPECIFIED' ) ;
#1244 = CYLINDRICAL_SURFACE ( 'NONE', #5248, 2.500999999999959922 ) ;
#1245 = DIRECTION ( 'NONE',  ( 1.000000000000000000, 0.000000000000000000, 0.000000000000000000 ) ) ;
#1246 = LOCAL_TIME ( 14, 11, 27.00000000000000000, #12563 ) ;
#1247 = APPROVAL ( #10846, 'UNSPECIFIED' ) ;
#1248 = FACE_OUTER_BOUND ( 'NONE', #3520, .T. ) ;
#1249 = CIRCLE ( 'NONE', #8089, 4.750000000000001776 ) ;
#1250 = EDGE_LOOP ( 'NONE', ( #1501, #11961, #11225, #22871 ) ) ;
#1251 = CARTESIAN_POINT ( 'NONE',  ( -20.00000000000000000, -20.00000000000000000, 8.000000000004559908 ) ) ;
#1252 = EDGE_CURVE ( 'NONE', #11510, #1465, #20380, .T. ) ;
#1253 = AXIS2_PLACEMENT_3D ( 'NONE', #17483, #4779, #22937 ) ;
#1254 = EDGE_CURVE ( 'NONE', #3206, #21066, #3725, .T. ) ;
#1255 = VECTOR ( 'NONE', #4328, 1000.000000000000000 ) ;
#1256 = CYLINDRICAL_SURFACE ( 'NONE', #5343, 2.500000000000000000 ) ;
#1257 = VERTEX_POINT ( 'NONE', #4196 ) ;
#1258 =( BOUNDED_CURVE ( )  B_SPLINE_CURVE ( 2, ( #13455, #15223, #2276 ),
 .UNSPECIFIED., .F., .F. ) 
 B_SPLINE_CURVE_WITH_KNOTS ( ( 3, 3 ),
 ( 0.000000000000000000, 0.5842180690389568998 ),
 .UNSPECIFIED. ) 
 CURVE ( )  GEOMETRIC_REPRESENTATION_ITEM ( )  RATIONAL_B_SPLINE_CURVE ( ( 1.000000000000000000, 1.154700538379249908, 1.000000000000000000 ) ) 
 REPRESENTATION_ITEM ( '' )  );
#1259 = CARTESIAN_POINT ( 'NONE',  ( 33.77164795278312681, 10.75935922908529996, -8.984920035094603463 ) ) ;
#1260 = DIRECTION ( 'NONE',  ( -0.9730401042858022320, 0.2306359803922080343, 5.959266323858941219E-17 ) ) ;
#1261 = ORIENTED_EDGE ( 'NONE', *, *, #22734, .T. ) ;
#1262 = DATE_TIME_ROLE ( 'classification_date' ) ;
#1263 = DIRECTION ( 'NONE',  ( 3.268868123706374574E-19, -6.243021194963094727E-17, -1.000000000000000000 ) ) ;
#1264 = ORIENTED_EDGE ( 'NONE', *, *, #2892, .F. ) ;
#1265 = AXIS2_PLACEMENT_3D ( 'NONE', #1825, #3618, #5398 ) ;
#1266 = ORIENTED_EDGE ( 'NONE', *, *, #241, .F. ) ;
#1267 = PERSON_AND_ORGANIZATION_ROLE ( 'design_owner' ) ;
#1268 = LINE ( 'NONE', #7100, #8065 ) ;
#1269 = APPROVAL_PERSON_ORGANIZATION ( #2293, #6762, #11598 ) ;
#1270 = CIRCLE ( 'NONE', #16075, 2.500000000000000444 ) ;
#1271 = ORIENTED_EDGE ( 'NONE', *, *, #12894, .F. ) ;
#1272 = LINE ( 'NONE', #19112, #3711 ) ;
#1273 = COORDINATED_UNIVERSAL_TIME_OFFSET ( 0, 0, .AHEAD. ) ;
#1274 = CIRCLE ( 'NONE', #3919, 4.250000000000000000 ) ;
#1275 = EDGE_CURVE ( 'NONE', #719, #23466, #12871, .T. ) ;
#1276 = AXIS2_PLACEMENT_3D ( 'NONE', #4483, #18628, #4128 ) ;
#1277 = APPROVAL_STATUS ( 'not_yet_approved' ) ;
#1278 = CARTESIAN_POINT ( 'NONE',  ( -31.64160538070510142, 6.334412527122569969, -5.000000000000000000 ) ) ;
#1279 = MANIFOLD_SOLID_BREP ( 'Imported1', #3817 ) ;
#1280 = EDGE_CURVE ( 'NONE', #21109, #18063, #11471, .T. ) ;
#1281 = VERTEX_POINT ( 'NONE', #153 ) ;
#1282 = EDGE_CURVE ( 'NONE', #22720, #13515, #20111, .T. ) ;
#1283 = VECTOR ( 'NONE', #11605, 1000.000000000000114 ) ;
#1284 = ADVANCED_FACE ( 'NONE', ( #3836 ), #2062, .T. ) ;
#1285 = EDGE_LOOP ( 'NONE', ( #14029, #10903, #7991, #3682 ) ) ;
#1286 = TOROIDAL_SURFACE ( 'NONE', #20269, 5.000000000000000000, 3.000000000000000000 ) ;
#1287 = DIRECTION ( 'NONE',  ( 1.000000000000000000, -2.099275139236451291E-23, -2.269747374248204951E-13 ) ) ;
#1288 = PLANE ( 'NONE',  #16185 ) ;
#1289 = EDGE_LOOP ( 'NONE', ( #838, #3310, #5505, #18636 ) ) ;
#1290 = LINE ( 'NONE', #21016, #1815 ) ;
#1291 = DIRECTION ( 'NONE',  ( -2.270069654138865127E-15, -1.000000000000000000, -4.574083617919690056E-30 ) ) ;
#1292 = CARTESIAN_POINT ( 'NONE',  ( 33.27705887009690144, -3.036156860537199798, -16.37500000000039790 ) ) ;
#1293 = ORIENTED_EDGE ( 'NONE', *, *, #4934, .F. ) ;
#1294 = ORIENTED_EDGE ( 'NONE', *, *, #1980, .T. ) ;
#1295 = FACE_BOUND ( 'NONE', #13599, .T. ) ;
#1296 = VERTEX_POINT ( 'NONE', #21999 ) ;
#1297 = PERSON_AND_ORGANIZATION ( #11966, #8758 ) ;
#1298 = ORIENTED_EDGE ( 'NONE', *, *, #657, .T. ) ;
#1299 = VERTEX_POINT ( 'NONE', #380 ) ;
#1300 = LINE ( 'NONE', #8565, #4668 ) ;
#1301 = APPROVAL_STATUS ( 'not_yet_approved' ) ;
#1302 = DIRECTION ( 'NONE',  ( -2.977235988022386522E-185, 9.605990953944227443E-124, 1.000000000000000000 ) ) ;
#1303 = CC_DESIGN_PERSON_AND_ORGANIZATION_ASSIGNMENT ( #3095, #20676, ( #4225 ) ) ;
#1304 = CARTESIAN_POINT ( 'NONE',  ( 118.5079952955230027, -6.794810348829399160, 15.50000000000000000 ) ) ;
#1305 = APPROVAL_ROLE ( '' ) ;
#1306 = PRODUCT_DEFINITION_SHAPE ( 'NONE', 'NONE',  #13884 ) ;
#1307 = VERTEX_POINT ( 'NONE', #14884 ) ;
#1308 = DIRECTION ( 'NONE',  ( -0.9730401042858022320, 0.2306359803922080343, 5.959266323858941219E-17 ) ) ;
#1309 = DIRECTION ( 'NONE',  ( -2.882701132343535037E-16, -9.096985413436440085E-33, 1.000000000000000000 ) ) ;
#1310 = ORIENTED_EDGE ( 'NONE', *, *, #12767, .T. ) ;
#1311 = MANIFOLD_SOLID_BREP ( 'Imported1', #20140 ) ;
#1312 = LINE ( 'NONE', #22806, #7881 ) ;
#1313 = FACE_BOUND ( 'NONE', #16135, .T. ) ;
#1314 = LINE ( 'NONE', #8581, #17932 ) ;
#1315 = ORIENTED_EDGE ( 'NONE', *, *, #5444, .F. ) ;
#1316 = CARTESIAN_POINT ( 'NONE',  ( -16.50000000000000000, -20.00000000000000000, 5.000000000000000000 ) ) ;
#1317 = AXIS2_PLACEMENT_3D ( 'NONE', #19326, #4958, #7734 ) ;
#1318 = PERSON_AND_ORGANIZATION ( #11966, #8758 ) ;
#1319 = EDGE_CURVE ( 'NONE', #11373, #16606, #10165, .T. ) ;
#1320 = ORIENTED_EDGE ( 'NONE', *, *, #19192, .T. ) ;
#1321 = ORIENTED_EDGE ( 'NONE', *, *, #8670, .F. ) ;
#1322 = DIRECTION ( 'NONE',  ( 0.000000000000000000, -1.000000000000000000, 0.000000000000000000 ) ) ;
#1323 = FACE_BOUND ( 'NONE', #15873, .T. ) ;
#1324 = DIRECTION ( 'NONE',  ( 0.9730401042858035643, -0.2306359803922028717, 2.804983810440357815E-16 ) ) ;
#1325 = APPROVAL_STATUS ( 'not_yet_approved' ) ;
#1326 = FACE_OUTER_BOUND ( 'NONE', #573, .T. ) ;
#1327 = FACE_OUTER_BOUND ( 'NONE', #2460, .T. ) ;
#1328 = DIRECTION ( 'NONE',  ( 0.9730401042858036753, -0.2306359803922028995, -5.959266323858677443E-17 ) ) ;
#1329 = DIRECTION ( 'NONE',  ( 1.000000000000000000, 0.000000000000000000, 0.000000000000000000 ) ) ;
#1330 = DIRECTION ( 'NONE',  ( 0.9730401042858024541, -0.2306359803922080898, -5.959266323858942451E-17 ) ) ;
#1331 = DATE_AND_TIME ( #21060, #7250 ) ;
#1332 = CARTESIAN_POINT ( 'NONE',  ( 35.65672502062392368, 7.704309056808580358, 8.774947752588879268 ) ) ;
#1333 = DIRECTION ( 'NONE',  ( 0.2306359803922037599, 0.9730401042858033422, -4.741332172908110825E-18 ) ) ;
#1334 = CARTESIAN_POINT ( 'NONE',  ( -65.82539143210260590, 12.65551411021120032, 5.000000000000000000 ) ) ;
#1335 = FACE_OUTER_BOUND ( 'NONE', #19472, .T. ) ;
#1336 = DIRECTION ( 'NONE',  ( 0.9999862922474493931, 0.005235963827108368503, 0.000000000000000000 ) ) ;
#1337 = VERTEX_POINT ( 'NONE', #15115 ) ;
#1338 = CARTESIAN_POINT ( 'NONE',  ( -62.84171802989940403, -5.847508446296020068, -7.200000000000000178 ) ) ;
#1339 = UNCERTAINTY_MEASURE_WITH_UNIT (LENGTH_MEASURE( 1.000000000000000082E-05 ), #22266, 'distance_accuracy_value', 'NONE');
#1340 = EDGE_CURVE ( 'NONE', #851, #22662, #11305, .T. ) ;
#1341 =( GEOMETRIC_REPRESENTATION_CONTEXT ( 3 ) GLOBAL_UNCERTAINTY_ASSIGNED_CONTEXT ( ( #13396 ) ) GLOBAL_UNIT_ASSIGNED_CONTEXT ( ( #9824, #11156, #18383 ) ) REPRESENTATION_CONTEXT ( 'NONE', 'WORKASPACE' ) );
#1342 = ORIENTED_EDGE ( 'NONE', *, *, #12866, .F. ) ;
#1343 = DIRECTION ( 'NONE',  ( 0.2306359803922017615, 0.9730401042858037863, -3.356987858687580135E-15 ) ) ;
#1344 = CARTESIAN_POINT ( 'NONE',  ( 36.57467860885130051, 21.71590586959139912, 15.00000000000000000 ) ) ;
#1345 = ORIENTED_EDGE ( 'NONE', *, *, #22589, .F. ) ;
#1346 = CC_DESIGN_DATE_AND_TIME_ASSIGNMENT ( #3174, #1262, ( #1162 ) ) ;
#1347 = LINE ( 'NONE', #5154, #18326 ) ;
#1348 = AXIS2_PLACEMENT_3D ( 'NONE', #633, #22359, #20603 ) ;
#1349 = MANIFOLD_SOLID_BREP ( 'Imported1', #19377 ) ;
#1350 = ORIENTED_EDGE ( 'NONE', *, *, #21538, .F. ) ;
#1351 = CARTESIAN_POINT ( 'NONE',  ( -4.514225866272930432, 4.676725866273569565, 5.000000000000000000 ) ) ;
#1352 = PERSON_AND_ORGANIZATION ( #11966, #8758 ) ;
#1353 = DIRECTION ( 'NONE',  ( -0.8511275218278966381, -0.5249589903860140128, 5.212440122911323074E-17 ) ) ;
#1354 = EDGE_CURVE ( 'NONE', #15994, #8200, #9793, .T. ) ;
#1355 = EDGE_CURVE ( 'NONE', #2977, #17755, #17491, .T. ) ;
#1356 = PLANE ( 'NONE',  #13399 ) ;
#1357 = FACE_OUTER_BOUND ( 'NONE', #5510, .T. ) ;
#1358 =( NAMED_UNIT ( * ) PLANE_ANGLE_UNIT ( ) SI_UNIT ( $, .RADIAN. ) );
#1359 = CARTESIAN_POINT ( 'NONE',  ( 36.30795141656459890, -8.893092097651951633, 18.00000000000000000 ) ) ;
#1360 = ORIENTED_EDGE ( 'NONE', *, *, #12888, .T. ) ;
#1361 = DIRECTION ( 'NONE',  ( 0.9999997101582432935, 0.0007613694435018768464, -1.641484103780244428E-33 ) ) ;
#1362 = VECTOR ( 'NONE', #19590, 1000.000000000000000 ) ;
#1363 = DESIGN_CONTEXT ( 'detailed design', #5520, 'design' ) ;
#1364 = DIRECTION ( 'NONE',  ( -0.2306359803922053142, -0.9730401042858028982, 0.000000000000000000 ) ) ;
#1365 = ORIENTED_EDGE ( 'NONE', *, *, #16593, .T. ) ;
#1366 = PLANE ( 'NONE',  #15411 ) ;
#1367 = CYLINDRICAL_SURFACE ( 'NONE', #4640, 3.500000000000000444 ) ;
#1368 = ORIENTED_EDGE ( 'NONE', *, *, #11010, .F. ) ;
#1369 = EDGE_CURVE ( 'NONE', #54, #17119, #4676, .T. ) ;
#1370 = CALENDAR_DATE ( 2026, 31, 10 ) ;
#1371 = LINE ( 'NONE', #5181, #7305 ) ;
#1372 = ORIENTED_EDGE ( 'NONE', *, *, #5950, .F. ) ;
#1373 = ORIENTED_EDGE ( 'NONE', *, *, #21584, .T. ) ;
#1375 = PERSON_AND_ORGANIZATION ( #11966, #8758 ) ;
#1374 = CC_DESIGN_PERSON_AND_ORGANIZATION_ASSIGNMENT ( #6363, #21077, ( #19087 ) ) ;
#1376 = CARTESIAN_POINT ( 'NONE',  ( 43.98050001724070057, -5.573152644851429471, -13.00000000000039968 ) ) ;
#1377 = ORIENTED_EDGE ( 'NONE', *, *, #9871, .T. ) ;
#1378 = AXIS2_PLACEMENT_3D ( 'NONE', #1986, #9243, #4005 ) ;
#1379 = CC_DESIGN_PERSON_AND_ORGANIZATION_ASSIGNMENT ( #9361, #16951, ( #19247 ) ) ;
#1380 = VECTOR ( 'NONE', #15366, 1000.000000000000000 ) ;
#1381 = CARTESIAN_POINT ( 'NONE',  ( -0.5391976746803449627, 18.33937061236850141, -7.621247264287879719E-15 ) ) ;
#1382 = SECURITY_CLASSIFICATION_LEVEL ( 'unclassified' ) ;
#1383 = EDGE_CURVE ( 'NONE', #3573, #22846, #17735, .T. ) ;
#1384 = EDGE_CURVE ( 'NONE', #7111, #12704, #14711, .T. ) ;
#1385 = EDGE_CURVE ( 'NONE', #15644, #2339, #5971, .T. ) ;
#1386 = DATE_AND_TIME ( #17434, #7278 ) ;
#1387 = DIRECTION ( 'NONE',  ( 0.005235963827121942714, -0.9999862922474493931, -2.738609489598291197E-14 ) ) ;
#1388 = SHAPE_REPRESENTATION ( '1602p_c_22', ( #12739 ), #15784 ) ;
#1389 = LINE ( 'NONE', #3298, #11151 ) ;
#1390 = EDGE_LOOP ( 'NONE', ( #11350, #21925 ) ) ;
#1391 = CIRCLE ( 'NONE', #19983, 4.250000000000000000 ) ;
#1392 = VECTOR ( 'NONE', #14982, 1000.000000000000000 ) ;
#1393 = EDGE_LOOP ( 'NONE', ( #6779, #6171 ) ) ;
#1394 = DIRECTION ( 'NONE',  ( 3.099353312215988811E-62, -1.534091707905539548E-92, -1.000000000000000000 ) ) ;
#1395 = DIRECTION ( 'NONE',  ( -0.02167246311338769799, 0.9997651245880698756, 0.000000000000000000 ) ) ;
#1396 = VERTEX_POINT ( 'NONE', #8236 ) ;
#1397 = EDGE_CURVE ( 'NONE', #14820, #13595, #4448, .T. ) ;
#1398 = LINE ( 'NONE', #6883, #5855 ) ;
#1399 = CARTESIAN_POINT ( 'NONE',  ( -24.50000000000000000, -30.47499999999999787, -21.50000000000000000 ) ) ;
#1400 = AXIS2_PLACEMENT_3D ( 'NONE', #2648, #2997, #22823 ) ;
#1401 = ORIENTED_EDGE ( 'NONE', *, *, #7316, .F. ) ;
#1402 = ORIENTED_EDGE ( 'NONE', *, *, #23017, .T. ) ;
#1403 = DIRECTION ( 'NONE',  ( -1.000000000000000000, 0.000000000000000000, 0.000000000000000000 ) ) ;
#1404 = ORIENTED_EDGE ( 'NONE', *, *, #2072, .T. ) ;
#1405 = DATE_TIME_ROLE ( 'creation_date' ) ;
#1406 = PERSON ( 'NAUO-PER15', 'UNSPECIFIED', 'UNSPECIFIED', ('UNSPECIFIED'), ('UNSPECIFIED'), ('UNSPECIFIED') ) ;
#1407 = ORIENTED_EDGE ( 'NONE', *, *, #18710, .T. ) ;
#1408 = VERTEX_POINT ( 'NONE', #6093 ) ;
#1409 = CARTESIAN_POINT ( 'NONE',  ( 38.63934541421534874, 19.58702556410829487, -13.00000000000029665 ) ) ;
#1410 = VECTOR ( 'NONE', #17002, 1000.000000000000227 ) ;
#1411 = COORDINATED_UNIVERSAL_TIME_OFFSET ( 0, 0, .AHEAD. ) ;
#1412 = EDGE_CURVE ( 'NONE', #4600, #645, #1790, .T. ) ;
#1413 = ADVANCED_FACE ( 'NONE', ( #20587 ), #20929, .T. ) ;
#1414 = AXIS2_PLACEMENT_3D ( 'NONE', #10896, #18361, #5170 ) ;
#1415 = AXIS2_PLACEMENT_3D ( 'NONE', #1710, #23433, #3374 ) ;
#1416 = CARTESIAN_POINT ( 'NONE',  ( -22.99999999999959854, -19.33065833018789803, 23.00000000000000000 ) ) ;
#1417 = AXIS2_PLACEMENT_3D ( 'NONE', #4886, #13553, #4526 ) ;
#1418 = LINE ( 'NONE', #12600, #14530 ) ;
#1419 = MECHANICAL_CONTEXT ( 'NONE', #2602, 'mechanical' ) ;
#1420 = ORIENTED_EDGE ( 'NONE', *, *, #5020, .F. ) ;
#1421 = VECTOR ( 'NONE', #17606, 1000.000000000000000 ) ;
#1422 = DIRECTION ( 'NONE',  ( 0.005235963827117092427, -0.9999862922474493931, -2.636227439667000721E-16 ) ) ;
#1423 = DIRECTION ( 'NONE',  ( -2.269700743865584947E-13, -2.220446049247695246E-15, -1.000000000000000000 ) ) ;
#1424 = EDGE_LOOP ( 'NONE', ( #7638, #12374, #2876, #22818, #17334 ) ) ;
#1425 = CIRCLE ( 'NONE', #22646, 5.000000000000000888 ) ;
#1426 = EDGE_CURVE ( 'NONE', #22280, #677, #7876, .T. ) ;
#1427 = LINE ( 'NONE', #5002, #660 ) ;
#1429 = CIRCLE ( 'NONE', #12082, 2.500000000000000888 ) ;
#1428 = DIRECTION ( 'NONE',  ( -1.000000000000000000, -6.662111140531837817E-09, 1.144917494144693313E-14 ) ) ;
#1430 = DIRECTION ( 'NONE',  ( 0.2306359803922053697, 0.9730401042858028982, 0.000000000000000000 ) ) ;
#1431 = ORIENTED_EDGE ( 'NONE', *, *, #11942, .T. ) ;
#1432 = FACE_BOUND ( 'NONE', #22637, .T. ) ;
#1433 = PERSON_AND_ORGANIZATION ( #11966, #8758 ) ;
#1434 = EDGE_LOOP ( 'NONE', ( #6714, #2606, #5028, #4099, #21342 ) ) ;
#1435 = EDGE_LOOP ( 'NONE', ( #8667, #19406, #11304, #9513, #2584, #18785 ) ) ;
#1436 = DIRECTION ( 'NONE',  ( -0.9999862922474492821, -0.005235963827121953122, 1.187304881134294758E-16 ) ) ;
#1437 = FACE_OUTER_BOUND ( 'NONE', #12122, .T. ) ;
#1438 = ADVANCED_FACE ( 'NONE', ( #2533 ), #2888, .T. ) ;
#1439 = CARTESIAN_POINT ( 'NONE',  ( -62.99678855639989905, 23.76850991288289805, -2.458499999999993690 ) ) ;
#1440 = CALENDAR_DATE ( 2026, 31, 10 ) ;
#1441 = EDGE_CURVE ( 'NONE', #1745, #16463, #9516, .T. ) ;
#1442 = CARTESIAN_POINT ( 'NONE',  ( 41.24356139695900225, 11.92996613406550033, -15.90000000000000036 ) ) ;
#1443 = LINE ( 'NONE', #15935, #15943 ) ;
#1444 = AXIS2_PLACEMENT_3D ( 'NONE', #17981, #1562, #3353 ) ;
#1445 = DIRECTION ( 'NONE',  ( 0.000000000000000000, 0.000000000000000000, 1.000000000000000000 ) ) ;
#1446 = ORIENTED_EDGE ( 'NONE', *, *, #19798, .F. ) ;
#1447 = DIRECTION ( 'NONE',  ( -0.1982893547227609354, -0.8365715274350927766, 0.5107146084542198983 ) ) ;
#1448 = APPROVAL_DATE_TIME ( #10623, #9908 ) ;
#1449 = CARTESIAN_POINT ( 'NONE',  ( -22.99995202268966921, -0.1204285676209190525, 2.500000000000000444 ) ) ;
#1450 = CARTESIAN_POINT ( 'NONE',  ( 34.50315935367051878, 10.80419468673720296, -27.44000000000050576 ) ) ;
#1451 = CARTESIAN_POINT ( 'NONE',  ( -72.77122628570259621, -6.881121833202230142, -0.01852613985921119921 ) ) ;
#1452 = CARTESIAN_POINT ( 'NONE',  ( 34.40556712239430226, 8.514986143071229918, 27.68999999999999773 ) ) ;
#1453 = CARTESIAN_POINT ( 'NONE',  ( -62.73971250800079957, -25.32895006819559924, -5.538452170245418869E-15 ) ) ;
#1454 = ORIENTED_EDGE ( 'NONE', *, *, #8240, .F. ) ;
#1455 = DIRECTION ( 'NONE',  ( -0.9730401042858022320, 0.2306359803922080343, 5.959266323858941219E-17 ) ) ;
#1456 = CC_DESIGN_PERSON_AND_ORGANIZATION_ASSIGNMENT ( #4552, #15720, ( #3463 ) ) ;
#1457 = CLOSED_SHELL ( 'NONE', ( #4208, #17229, #17531, #19358, #21249, #2265 ) ) ;
#1458 = ORIENTED_EDGE ( 'NONE', *, *, #5679, .F. ) ;
#1459 = CARTESIAN_POINT ( 'NONE',  ( 33.94234173009040489, 21.44981837135919989, -12.50000000000050093 ) ) ;
#1460 = AXIS2_PLACEMENT_3D ( 'NONE', #5786, #20157, #10806 ) ;
#1461 = DIRECTION ( 'NONE',  ( 0.000000000000000000, 0.000000000000000000, -1.000000000000000000 ) ) ;
#1462 = VERTEX_POINT ( 'NONE', #17383 ) ;
#1463 = CARTESIAN_POINT ( 'NONE',  ( 31.49315201223960159, -2.613324229818040134, 14.15470053837944953 ) ) ;
#1464 = MANIFOLD_SOLID_BREP ( 'Imported1', #19014 ) ;
#1465 = VERTEX_POINT ( 'NONE', #6226 ) ;
#1466 = DIRECTION ( 'NONE',  ( 0.2306359803922040652, 0.9730401042858032312, -4.849856555169149244E-15 ) ) ;
#1467 = CALENDAR_DATE ( 2026, 31, 10 ) ;
#1468 = CARTESIAN_POINT ( 'NONE',  ( 43.14167273007649328, 18.99928136731766770, -13.00000000000000000 ) ) ;
#1469 = CARTESIAN_POINT ( 'NONE',  ( 61.55522920193588021, -1.517168634553750062, 1.006920016453334892E-14 ) ) ;
#1470 = ADVANCED_FACE ( 'NONE', ( #13469 ), #20703, .T. ) ;
#1471 = CARTESIAN_POINT ( 'NONE',  ( 34.40556712239440174, 8.514986143070949254, -27.69000000000049866 ) ) ;
#1472 = PERSON_AND_ORGANIZATION_ROLE ( 'design_owner' ) ;
#1473 = LINE ( 'NONE', #7312, #6614 ) ;
#1474 = ORIENTED_EDGE ( 'NONE', *, *, #323, .F. ) ;
#1475 = CARTESIAN_POINT ( 'NONE',  ( 113.4570673249340018, -28.10438863268850085, 3.399999999999999911 ) ) ;
#1476 = DIRECTION ( 'NONE',  ( -0.9730401042858046745, 0.2306359803921981810, 0.000000000000000000 ) ) ;
#1477 = ORIENTED_EDGE ( 'NONE', *, *, #11222, .T. ) ;
#1478 = APPROVAL_PERSON_ORGANIZATION ( #17268, #8513, #10044 ) ;
#1479 = CARTESIAN_POINT ( 'NONE',  ( 34.62304412778976825, 11.60439875761490747, -8.864945788362616597 ) ) ;
#1480 = AXIS2_PLACEMENT_3D ( 'NONE', #15233, #22343, #13342 ) ;
#1481 = DIRECTION ( 'NONE',  ( 0.9730401042858036753, -0.2306359803922031493, 2.740969466505752002E-16 ) ) ;
#1482 = EDGE_CURVE ( 'NONE', #14624, #2629, #9910, .T. ) ;
#1483 = EDGE_CURVE ( 'NONE', #21214, #404, #860, .T. ) ;
#1484 = ORIENTED_EDGE ( 'NONE', *, *, #14448, .F. ) ;
#1485 = DIRECTION ( 'NONE',  ( 0.9730401042858024541, -0.2306359803922080898, -5.959266323858952312E-17 ) ) ;
#1486 = ORIENTED_EDGE ( 'NONE', *, *, #19639, .F. ) ;
#1487 = EDGE_LOOP ( 'NONE', ( #19660, #19635, #15276, #12559 ) ) ;
#1488 = DATE_AND_TIME ( #21454, #17888 ) ;
#1489 = CYLINDRICAL_SURFACE ( 'NONE', #9583, 4.250000000000000000 ) ;
#1490 = ORIENTED_EDGE ( 'NONE', *, *, #5146, .F. ) ;
#1491 = DIRECTION ( 'NONE',  ( -0.9997648975362233292, -0.02168293463498000007, 0.000000000000000000 ) ) ;
#1492 = APPROVAL_DATE_TIME ( #23346, #947 ) ;
#1493 = PRODUCT_DEFINITION_SHAPE ( 'NONE', 'NONE',  #14615 ) ;
#1494 = COORDINATED_UNIVERSAL_TIME_OFFSET ( 0, 0, .AHEAD. ) ;
#1495 = AXIS2_PLACEMENT_3D ( 'NONE', #9711, #647, #14917 ) ;
#1496 = CARTESIAN_POINT ( 'NONE',  ( -65.64475015647069256, -21.84411297095480009, 5.000000000000000000 ) ) ;
#1497 = AXIS2_PLACEMENT_3D ( 'NONE', #461, #7728, #13192 ) ;
#1498 = EDGE_CURVE ( 'NONE', #10008, #5968, #9119, .T. ) ;
#1499 = TOROIDAL_SURFACE ( 'NONE', #8729, 3.750000000000000000, 0.5000000000000000000 ) ;
#1500 = DIRECTION ( 'NONE',  ( 0.000000000000000000, 0.000000000000000000, -1.000000000000000000 ) ) ;
#1501 = ORIENTED_EDGE ( 'NONE', *, *, #20404, .T. ) ;
#1502 = APPROVAL ( #8178, 'UNKNOWN' ) ;
#1503 = CC_DESIGN_DATE_AND_TIME_ASSIGNMENT ( #22819, #22940, ( #16907 ) ) ;
#1504 = ORIENTED_EDGE ( 'NONE', *, *, #2070, .F. ) ;
#1505 = DIRECTION ( 'NONE',  ( 0.9730401042858036753, -0.2306359803922028995, -5.432877459303547669E-17 ) ) ;
#1506 = LINE ( 'NONE', #8425, #5948 ) ;
#1507 = ORIENTED_EDGE ( 'NONE', *, *, #7243, .F. ) ;
#1508 = EDGE_CURVE ( 'NONE', #10900, #22391, #8479, .T. ) ;
#1509 = EDGE_CURVE ( 'NONE', #21424, #16953, #17974, .T. ) ;
#1510 = PRODUCT_DEFINITION_FORMATION_WITH_SPECIFIED_SOURCE ( 'ANY', '', #10832, .NOT_KNOWN. ) ;
#1511 = DIRECTION ( 'NONE',  ( 2.086281924601080239E-16, 1.946516371809877606E-18, -1.000000000000000000 ) ) ;
#1512 = CARTESIAN_POINT ( 'NONE',  ( -16.50000000000000000, -20.00000000000000000, 2.500000000000000000 ) ) ;
#1513 = ORIENTED_EDGE ( 'NONE', *, *, #33, .F. ) ;
#1514 = ORIENTED_EDGE ( 'NONE', *, *, #13472, .F. ) ;
#1515 = AXIS2_PLACEMENT_3D ( 'NONE', #10906, #1842, #16448 ) ;
#1516 = CALENDAR_DATE ( 2026, 31, 10 ) ;
#1517 = ORIENTED_EDGE ( 'NONE', *, *, #9574, .F. ) ;
#1518 = ORIENTED_EDGE ( 'NONE', *, *, #13071, .F. ) ;
#1519 = CARTESIAN_POINT ( 'NONE',  ( 5.000000000000000000, -30.47499999999999787, -19.00000000000000000 ) ) ;
#1520 = APPROVAL_ROLE ( '' ) ;
#1521 = VECTOR ( 'NONE', #2978, 999.9999999999998863 ) ;
#1522 = DIRECTION ( 'NONE',  ( -0.9730401042858035643, 0.2306359803922028717, 5.958148513035547083E-17 ) ) ;
#1523 = APPROVAL_STATUS ( 'not_yet_approved' ) ;
#1524 =( BOUNDED_CURVE ( )  B_SPLINE_CURVE ( 2, ( #13608, #8157, #22733 ),
 .UNSPECIFIED., .F., .F. ) 
 B_SPLINE_CURVE_WITH_KNOTS ( ( 3, 3 ),
 ( 0.2928548593876180162, 0.5857097187752360323 ),
 .UNSPECIFIED. ) 
 CURVE ( )  GEOMETRIC_REPRESENTATION_ITEM ( )  RATIONAL_B_SPLINE_CURVE ( ( 1.000000000000000000, 1.037954849302029858, 1.000000000000000000 ) ) 
 REPRESENTATION_ITEM ( '' )  );
#1525 = VECTOR ( 'NONE', #3468, 1000.000000000000000 ) ;
#1526 = EDGE_CURVE ( 'NONE', #4592, #10583, #1443, .T. ) ;
#1527 = SECURITY_CLASSIFICATION ( '', '', #2523 ) ;
#1528 = APPROVAL_PERSON_ORGANIZATION ( #7889, #2920, #20470 ) ;
#1529 = LINE ( 'NONE', #23269, #4299 ) ;
#1530 = PRODUCT_DEFINITION ( 'UNKNOWN', '', #1997, #14428 ) ;
#1531 = DATE_AND_TIME ( #23031, #23176 ) ;
#1532 = CC_DESIGN_DATE_AND_TIME_ASSIGNMENT ( #13309, #5833, ( #8957 ) ) ;
#1533 = ORIENTED_EDGE ( 'NONE', *, *, #10404, .T. ) ;
#1534 = FACE_OUTER_BOUND ( 'NONE', #19911, .T. ) ;
#1535 = DIRECTION ( 'NONE',  ( 6.123230199561449365E-17, 4.868008300101910084E-15, 1.000000000000000000 ) ) ;
#1536 = CIRCLE ( 'NONE', #14063, 3.499999999999999112 ) ;
#1537 = ORIENTED_EDGE ( 'NONE', *, *, #16483, .T. ) ;
#1538 = ADVANCED_FACE ( 'NONE', ( #21280 ), #17622, .F. ) ;
#1539 = ADVANCED_FACE ( 'NONE', ( #10739 ), #3797, .T. ) ;
#1540 = DIRECTION ( 'NONE',  ( 0.1177891644214439926, 0.4969457958704997513, -0.8597503060258446794 ) ) ;
#1541 = DIRECTION ( 'NONE',  ( -0.9999862922474492821, -0.005235963827121953122, 1.187304881134294758E-16 ) ) ;
#1542 = CARTESIAN_POINT ( 'NONE',  ( -24.50000000000000000, -31.09999999999999787, -19.00000000000000000 ) ) ;
#1543 = ORIENTED_EDGE ( 'NONE', *, *, #16093, .F. ) ;
#1544 = VERTEX_POINT ( 'NONE', #10618 ) ;
#1545 = CARTESIAN_POINT ( 'NONE',  ( 45.07211867146829576, 28.08243186520855161, 15.99999999999969802 ) ) ;
#1546 = APPROVAL_ROLE ( '' ) ;
#1547 = LOCAL_TIME ( 14, 11, 27.00000000000000000, #9511 ) ;
#1548 = EDGE_LOOP ( 'NONE', ( #18129, #6141, #23227, #20317, #3227 ) ) ;
#1549 = ORIENTED_EDGE ( 'NONE', *, *, #19877, .T. ) ;
#1550 = LINE ( 'NONE', #21502, #5395 ) ;
#1551 = CARTESIAN_POINT ( 'NONE',  ( 30.57814311865390167, -3.583136841839989817, 11.00000000000019895 ) ) ;
#1552 = LOCAL_TIME ( 14, 11, 27.00000000000000000, #20821 ) ;
#1553 = LINE ( 'NONE', #17616, #5745 ) ;
#1554 = DATE_AND_TIME ( #17842, #9193 ) ;
#1555 = DIRECTION ( 'NONE',  ( -1.304396158928310329E-15, -5.761557392270100456E-15, 1.000000000000000000 ) ) ;
#1556 = APPROVAL_PERSON_ORGANIZATION ( #8748, #12270, #21334 ) ;
#1557 = CARTESIAN_POINT ( 'NONE',  ( 5.000000000000000000, -31.09999999999999787, -2.500000000000000000 ) ) ;
#1558 = SECURITY_CLASSIFICATION ( '', '', #2090 ) ;
#1559 =( REPRESENTATION_RELATIONSHIP ('NONE','NONE', #18771, #19303 ) REPRESENTATION_RELATIONSHIP_WITH_TRANSFORMATION ( #16899 )SHAPE_REPRESENTATION_RELATIONSHIP( ) );
#1560 = EDGE_CURVE ( 'NONE', #10900, #21046, #7052, .T. ) ;
#1561 = DIRECTION ( 'NONE',  ( 1.000000000000000000, 0.000000000000000000, 0.000000000000000000 ) ) ;
#1562 = DIRECTION ( 'NONE',  ( 0.9730401042858035643, -0.2306359803922028717, -5.432877459303547053E-17 ) ) ;
#1563 = COORDINATED_UNIVERSAL_TIME_OFFSET ( 0, 0, .AHEAD. ) ;
#1564 = CC_DESIGN_APPROVAL ( #6450, ( #22038 ) ) ;
#1565 = LINE ( 'NONE', #10749, #4566 ) ;
#1566 = DIRECTION ( 'NONE',  ( -1.000000000000000000, 2.270069654138870255E-15, -3.099353312215989243E-62 ) ) ;
#1567 = EDGE_CURVE ( 'NONE', #22209, #6518, #19393, .T. ) ;
#1568 = AXIS2_PLACEMENT_3D ( 'NONE', #19387, #12390, #17841 ) ;
#1569 = CARTESIAN_POINT ( 'NONE',  ( 31.56827854690379098, -0.8510906712621758574, 14.00000000000018296 ) ) ;
#1570 = DIRECTION ( 'NONE',  ( 0.000000000000000000, -1.554450629062379680E-16, 1.000000000000000000 ) ) ;
#1571 = ADVANCED_FACE ( 'NONE', ( #1327, #8828 ), #23297, .T. ) ;
#1572 = FACE_OUTER_BOUND ( 'NONE', #16686, .T. ) ;
#1573 = VERTEX_POINT ( 'NONE', #17845 ) ;
#1574 = CC_DESIGN_APPROVAL ( #10821, ( #13727 ) ) ;
#1575 = FACE_BOUND ( 'NONE', #10925, .T. ) ;
#1576 = UNCERTAINTY_MEASURE_WITH_UNIT (LENGTH_MEASURE( 1.000000000000000082E-05 ), #9687, 'distance_accuracy_value', 'NONE');
#1577 = ORIENTED_EDGE ( 'NONE', *, *, #14549, .T. ) ;
#1578 = DIRECTION ( 'NONE',  ( 0.000000000000000000, 1.156482317317871478E-16, 1.000000000000000000 ) ) ;
#1579 = LINE ( 'NONE', #12410, #8740 ) ;
#1580 = VERTEX_POINT ( 'NONE', #6933 ) ;
#1581 = MANIFOLD_SOLID_BREP ( 'Imported1', #2227 ) ;
#1582 = EDGE_LOOP ( 'NONE', ( #23157, #15156 ) ) ;
#1583 = LOCAL_TIME ( 14, 11, 27.00000000000000000, #10737 ) ;
#1584 = CARTESIAN_POINT ( 'NONE',  ( 34.89491389100810181, 23.30074776265909975, -13.00000000000049916 ) ) ;
#1585 = APPROVAL_STATUS ( 'not_yet_approved' ) ;
#1586 = VECTOR ( 'NONE', #21926, 1000.000000000000000 ) ;
#1587 = FACE_OUTER_BOUND ( 'NONE', #17448, .T. ) ;
#1588 = AXIS2_PLACEMENT_3D ( 'NONE', #7935, #15165, #20643 ) ;
#1589 = CC_DESIGN_APPROVAL ( #12836, ( #22778 ) ) ;
#1590 = DIRECTION ( 'NONE',  ( -0.9730401042858024541, 0.2306359803922080898, 5.959266323858942451E-17 ) ) ;
#1591 = PRODUCT_DEFINITION ( 'UNKNOWN', '', #7231, #1832 ) ;
#1592 = AXIS2_PLACEMENT_3D ( 'NONE', #2985, #8583, #4773 ) ;
#1593 = FACE_OUTER_BOUND ( 'NONE', #6313, .T. ) ;
#1594 = DIRECTION ( 'NONE',  ( 1.000000000000000000, 0.000000000000000000, 0.000000000000000000 ) ) ;
#1595 = EDGE_CURVE ( 'NONE', #17959, #4383, #18222, .T. ) ;
#1596 = DIRECTION ( 'NONE',  ( 0.9730401042858035643, -0.2306359803922028717, -5.958148513035547083E-17 ) ) ;
#1597 = DIRECTION ( 'NONE',  ( -1.000000000000000000, 0.000000000000000000, 0.000000000000000000 ) ) ;
#1598 = CARTESIAN_POINT ( 'NONE',  ( -19.49999999982360066, -0.1021026942259700004, -1.101737663870589950E-14 ) ) ;
#1599 = PRODUCT_DEFINITION_FORMATION_WITH_SPECIFIED_SOURCE ( 'ANY', '', #10100, .NOT_KNOWN. ) ;
#1600 = LINE ( 'NONE', #21089, #733 ) ;
#1601 = EDGE_LOOP ( 'NONE', ( #17670, #11463 ) ) ;
#1602 = CARTESIAN_POINT ( 'NONE',  ( 34.03002896453733683, 19.65184737158733341, -13.00000000000049916 ) ) ;
#1603 = VECTOR ( 'NONE', #18915, 1000.000000000000227 ) ;
#1604 = DIRECTION ( 'NONE',  ( 0.000000000000000000, 0.000000000000000000, -1.000000000000000000 ) ) ;
#1605 = AXIS2_PLACEMENT_3D ( 'NONE', #402, #3982, #19909 ) ;
#1606 = ORIENTED_EDGE ( 'NONE', *, *, #18199, .T. ) ;
#1607 = DIRECTION ( 'NONE',  ( 0.1997366180463769070, 0.8426774492125652660, 0.5000000000000003331 ) ) ;
#1608 = VERTEX_POINT ( 'NONE', #5137 ) ;
#1609 = VERTEX_POINT ( 'NONE', #6808 ) ;
#1610 = COORDINATED_UNIVERSAL_TIME_OFFSET ( 0, 0, .AHEAD. ) ;
#1611 = CIRCLE ( 'NONE', #16790, 3.499999999999999556 ) ;
#1612 = FACE_OUTER_BOUND ( 'NONE', #3859, .T. ) ;
#1613 = EDGE_CURVE ( 'NONE', #12681, #21263, #15176, .T. ) ;
#1614 = ORIENTED_EDGE ( 'NONE', *, *, #15520, .F. ) ;
#1615 = FACE_OUTER_BOUND ( 'NONE', #12145, .T. ) ;
#1616 = AXIS2_PLACEMENT_3D ( 'NONE', #21479, #200, #1872 ) ;
#1617 = CALENDAR_DATE ( 2026, 31, 10 ) ;
#1618 = CONICAL_SURFACE ( 'NONE', #20970, 2.624999999999998668, 0.4636476090008101458 ) ;
#1619 = LOCAL_TIME ( 14, 11, 27.00000000000000000, #16563 ) ;
#1620 = DATE_AND_TIME ( #3403, #6904 ) ;
#1621 = CARTESIAN_POINT ( 'NONE',  ( 39.27359436029428963, 22.26288585089417538, -17.25000000000050093 ) ) ;
#1622 = AXIS2_PLACEMENT_3D ( 'NONE', #11661, #22434, #16729 ) ;
#1623 = AXIS2_PLACEMENT_3D ( 'NONE', #20579, #11589, #18816 ) ;
#1624 = VECTOR ( 'NONE', #2774, 1000.000000000000000 ) ;
#1625 = DIRECTION ( 'NONE',  ( -1.000000000000000000, -6.662112528310618598E-09, 2.269018306577664942E-13 ) ) ;
#1626 = ORIENTED_EDGE ( 'NONE', *, *, #11578, .T. ) ;
#1627 = FACE_OUTER_BOUND ( 'NONE', #13311, .T. ) ;
#1628 = ORIENTED_EDGE ( 'NONE', *, *, #9085, .T. ) ;
#1629 = VECTOR ( 'NONE', #7769, 1000.000000000000114 ) ;
#1630 = DIRECTION ( 'NONE',  ( 0.000000000000000000, 1.000000000000000000, 0.000000000000000000 ) ) ;
#1631 = CARTESIAN_POINT ( 'NONE',  ( -21.99941224366415682, -0.1563100308134250105, -2.500000000000000000 ) ) ;
#1632 = VERTEX_POINT ( 'NONE', #21509 ) ;
#1633 = CC_DESIGN_SECURITY_CLASSIFICATION ( #17596, ( #23476 ) ) ;
#1634 = VECTOR ( 'NONE', #15146, 999.9999999999998863 ) ;
#1635 = CARTESIAN_POINT ( 'NONE',  ( 35.59419854219520118, 9.774809681453540122, 26.50000000000000000 ) ) ;
#1636 = DIRECTION ( 'NONE',  ( -0.9997648975362222190, -0.02168293463503410262, 0.000000000000000000 ) ) ;
#1637 = VERTEX_POINT ( 'NONE', #12289 ) ;
#1638 = CIRCLE ( 'NONE', #3163, 3.499999999999998668 ) ;
#1639 = ORIENTED_EDGE ( 'NONE', *, *, #2781, .F. ) ;
#1640 = CALENDAR_DATE ( 2026, 31, 10 ) ;
#1641 = EDGE_CURVE ( 'NONE', #16103, #3586, #12506, .T. ) ;
#1642 = ORIENTED_EDGE ( 'NONE', *, *, #18644, .F. ) ;
#1643 = CONICAL_SURFACE ( 'NONE', #10786, 1.154700538379250796, 1.047197551196598297 ) ;
#1644 = VERTEX_POINT ( 'NONE', #8942 ) ;
#1645 = DIRECTION ( 'NONE',  ( -0.2306359803922019835, -0.9730401042858037863, 4.857225732735059075E-15 ) ) ;
#1646 = APPLICATION_PROTOCOL_DEFINITION ( 'international standard', 'config_control_design', 1994, #328 ) ;
#1647 = CC_DESIGN_PERSON_AND_ORGANIZATION_ASSIGNMENT ( #16929, #11265, ( #13355 ) ) ;
#1648 = LINE ( 'NONE', #10236, #7807 ) ;
#1649 = DATE_TIME_ROLE ( 'classification_date' ) ;
#1650 = EDGE_CURVE ( 'NONE', #3196, #15865, #10501, .T. ) ;
#1651 = ADVANCED_FACE ( 'NONE', ( #16170 ), #12629, .T. ) ;
#1652 = AXIS2_PLACEMENT_3D ( 'NONE', #2656, #2183, #4339 ) ;
#1653 =( LENGTH_UNIT ( ) NAMED_UNIT ( * ) SI_UNIT ( .MILLI., .METRE. ) );
#1654 = DIRECTION ( 'NONE',  ( 0.9730401042858035643, -0.2306359803922028717, -5.432877459303547053E-17 ) ) ;
#1655 = AXIS2_PLACEMENT_3D ( 'NONE', #10487, #12609, #19850 ) ;
#1656 = PERSON_AND_ORGANIZATION_ROLE ( 'classification_officer' ) ;
#1657 = EDGE_CURVE ( 'NONE', #6574, #7703, #12395, .T. ) ;
#1658 = ORIENTED_EDGE ( 'NONE', *, *, #19611, .T. ) ;
#1659 = FACE_OUTER_BOUND ( 'NONE', #16445, .T. ) ;
#1660 = DIRECTION ( 'NONE',  ( -6.662111338785949120E-09, 1.000000000000000000, -1.982541115402066096E-15 ) ) ;
#1661 = ORIENTED_EDGE ( 'NONE', *, *, #14192, .F. ) ;
#1662 = DIRECTION ( 'NONE',  ( -0.9907450477976873504, 0.000000000000000000, -0.1357359578901564667 ) ) ;
#1663 = DIRECTION ( 'NONE',  ( -3.210834492181045054E-17, 2.441916418604795262E-15, 1.000000000000000000 ) ) ;
#1664 = PLANE ( 'NONE',  #13759 ) ;
#1665 = ORIENTED_EDGE ( 'NONE', *, *, #19845, .T. ) ;
#1666 = ORIENTED_EDGE ( 'NONE', *, *, #16477, .F. ) ;
#1667 = CARTESIAN_POINT ( 'NONE',  ( 46.46175228317039796, -6.161274394849590053, -13.00000000000000000 ) ) ;
#1668 = ORIENTED_EDGE ( 'NONE', *, *, #8798, .T. ) ;
#1669 = PERSON_AND_ORGANIZATION ( #11966, #8758 ) ;
#1670 = EDGE_CURVE ( 'NONE', #19937, #21288, #7163, .T. ) ;
#1671 = ORIENTED_EDGE ( 'NONE', *, *, #4604, .F. ) ;
#1672 = ORIENTED_EDGE ( 'NONE', *, *, #13792, .F. ) ;
#1673 = DIRECTION ( 'NONE',  ( 0.000000000000000000, 0.000000000000000000, 1.000000000000000000 ) ) ;
#1674 = CARTESIAN_POINT ( 'NONE',  ( -27.00000000000000000, -30.47499999999999787, 19.00000000000000000 ) ) ;
#1675 =( BOUNDED_CURVE ( )  B_SPLINE_CURVE ( 2, ( #6572, #15462, #19165 ),
 .UNSPECIFIED., .F., .F. ) 
 B_SPLINE_CURVE_WITH_KNOTS ( ( 3, 3 ),
 ( 0.000000000000000000, 0.2336872276155859962 ),
 .UNSPECIFIED. ) 
 CURVE ( )  GEOMETRIC_REPRESENTATION_ITEM ( )  RATIONAL_B_SPLINE_CURVE ( ( 1.000000000000000000, 1.154700538379249908, 1.000000000000000000 ) ) 
 REPRESENTATION_ITEM ( '' )  );
#1676 = DIRECTION ( 'NONE',  ( 0.000000000000000000, 0.000000000000000000, 1.000000000000000000 ) ) ;
#1677 = APPROVAL_STATUS ( 'not_yet_approved' ) ;
#1678 = CARTESIAN_POINT ( 'NONE',  ( -20.00000000000000000, -22.50000000000000000, 5.500000000004564349 ) ) ;
#1679 = CC_DESIGN_DATE_AND_TIME_ASSIGNMENT ( #21678, #7000, ( #2395 ) ) ;
#1680 = APPROVAL ( #16362, 'UNSPECIFIED' ) ;
#1681 = DIRECTION ( 'NONE',  ( -8.911056267098788616E-18, -1.998401444326210262E-15, -1.000000000000000000 ) ) ;
#1682 = EDGE_CURVE ( 'NONE', #22814, #7235, #5366, .T. ) ;
#1683 = EDGE_CURVE ( 'NONE', #13022, #13532, #20116, .T. ) ;
#1684 = CC_DESIGN_PERSON_AND_ORGANIZATION_ASSIGNMENT ( #4142, #102, ( #4882 ) ) ;
#1685 = DIRECTION ( 'NONE',  ( 1.000000000000000000, 0.000000000000000000, 0.000000000000000000 ) ) ;
#1686 = CARTESIAN_POINT ( 'NONE',  ( 118.6002496876800052, -6.405594307115129560, 18.89999999999999858 ) ) ;
#1687 = APPROVAL_ROLE ( '' ) ;
#1688 = LINE ( 'NONE', #9534, #8746 ) ;
#1689 = DIRECTION ( 'NONE',  ( -0.4865200521429013936, 0.1153179901961013387, -0.8660254037844388186 ) ) ;
#1690 = APPLICATION_CONTEXT ( 'configuration controlled 3d designs of mechanical parts and assemblies' ) ;
#1691 = DIRECTION ( 'NONE',  ( 0.000000000000000000, -1.000000000000000000, 1.998401444326210262E-15 ) ) ;
#1692 = DIRECTION ( 'NONE',  ( -5.964507377817269296E-17, -4.861311874385510251E-15, -1.000000000000000000 ) ) ;
#1693 = DIRECTION ( 'NONE',  ( 0.000000000000000000, -1.000000000000000000, 2.081668171172168119E-15 ) ) ;
#1694 = VERTEX_POINT ( 'NONE', #20212 ) ;
#1695 = CARTESIAN_POINT ( 'NONE',  ( 36.43025397111700414, 13.30208005948929895, -26.50000000000049738 ) ) ;
#1696 = EDGE_CURVE ( 'NONE', #1911, #2422, #14515, .T. ) ;
#1697 = PRODUCT ( '1602p_c_41', '1602p_c_41', '', ( #2016 ) ) ;
#1698 = EDGE_LOOP ( 'NONE', ( #2794, #17614, #14991, #6792 ) ) ;
#1699 = CARTESIAN_POINT ( 'NONE',  ( 54.98564867634340203, -10.30593110903627441, -13.00000000000000000 ) ) ;
#1700 = CARTESIAN_POINT ( 'NONE',  ( -20.00000000000190070, -20.00000000000000000, -8.499999999995459632 ) ) ;
#1701 = EDGE_LOOP ( 'NONE', ( #19939, #14934, #11313, #2927 ) ) ;
#1702 = CARTESIAN_POINT ( 'NONE',  ( -62.73971250800079957, -25.32895006819559924, -5.538452170245418869E-15 ) ) ;
#1703 = EDGE_CURVE ( 'NONE', #7758, #10964, #18189, .T. ) ;
#1704 = ADVANCED_BREP_SHAPE_REPRESENTATION ( '', ( #16939, #12739 ), #21233 ) ;
#1705 = MANIFOLD_SOLID_BREP ( 'Boss-Extrude2', #10594 ) ;
#1706 = ORIENTED_EDGE ( 'NONE', *, *, #22263, .T. ) ;
#1707 = VECTOR ( 'NONE', #2009, 1000.000000000000000 ) ;
#1708 = FACE_OUTER_BOUND ( 'NONE', #20836, .T. ) ;
#1709 = MECHANICAL_CONTEXT ( 'NONE', #7460, 'mechanical' ) ;
#1710 = CARTESIAN_POINT ( 'NONE',  ( -12.59661859123080063, -1.225550774622850225, -7.999999999997189803 ) ) ;
#1711 = ADVANCED_FACE ( 'NONE', ( #477 ), #5705, .F. ) ;
#1712 = EDGE_CURVE ( 'NONE', #7633, #13130, #7990, .T. ) ;
#1713 =( NAMED_UNIT ( * ) PLANE_ANGLE_UNIT ( ) SI_UNIT ( $, .RADIAN. ) );
#1714 = DIRECTION ( 'NONE',  ( -4.033639808943980242E-37, 5.936300330036069670E-19, -1.000000000000000000 ) ) ;
#1715 = DIRECTION ( 'NONE',  ( -0.2306359803921919083, -0.9730401042858062288, -4.336808689942036669E-14 ) ) ;
#1716 = DIRECTION ( 'NONE',  ( 3.099353312215988811E-62, -1.534091707905539548E-92, -1.000000000000000000 ) ) ;
#1717 = CARTESIAN_POINT ( 'NONE',  ( 33.37436288052550282, -3.059220458576299873, 13.00000000000019895 ) ) ;
#1718 = CARTESIAN_POINT ( 'NONE',  ( -16.50000000000000000, -20.00000000000000000, 1.084773659275596300E-61 ) ) ;
#1719 = FACE_OUTER_BOUND ( 'NONE', #13019, .T. ) ;
#1720 = ORIENTED_EDGE ( 'NONE', *, *, #8269, .T. ) ;
#1721 = PLANE ( 'NONE',  #20625 ) ;
#1722 = CARTESIAN_POINT ( 'NONE',  ( 13.44924913854525883, 13.96160742853852099, -3.505536662654785132E-15 ) ) ;
#1723 = EDGE_LOOP ( 'NONE', ( #6665, #14228, #3502, #23115 ) ) ;
#1724 = DATE_AND_TIME ( #12217, #9546 ) ;
#1725 = DIRECTION ( 'NONE',  ( -0.9730401042858036753, 0.2306359803922023999, -1.110223024625155524E-17 ) ) ;
#1726 = ORIENTED_EDGE ( 'NONE', *, *, #10182, .T. ) ;
#1727 = PERSON_AND_ORGANIZATION ( #11966, #8758 ) ;
#1728 = CARTESIAN_POINT ( 'NONE',  ( -20.00000000397270128, 22.95208919257159863, 5.500000000004459544 ) ) ;
#1729 = EDGE_CURVE ( 'NONE', #9507, #22544, #12846, .T. ) ;
#1730 = EDGE_LOOP ( 'NONE', ( #5320, #15794 ) ) ;
#1731 = CARTESIAN_POINT ( 'NONE',  ( -19.99975861755289941, 22.95209442650110176, 3.749999999999949818 ) ) ;
#1732 = DATE_AND_TIME ( #9227, #9995 ) ;
#1733 = ADVANCED_FACE ( 'NONE', ( #7738 ), #9165, .T. ) ;
#1734 =( GEOMETRIC_REPRESENTATION_CONTEXT ( 3 ) GLOBAL_UNCERTAINTY_ASSIGNED_CONTEXT ( ( #1576 ) ) GLOBAL_UNIT_ASSIGNED_CONTEXT ( ( #9687, #15004, #7886 ) ) REPRESENTATION_CONTEXT ( 'NONE', 'WORKASPACE' ) );
#1735 = SHAPE_REPRESENTATION ( '1602p_c_46', ( #12739 ), #15185 ) ;
#1736 = CARTESIAN_POINT ( 'NONE',  ( -68.51547434528259828, -24.91260405369630249, -2.885287058652779450E-14 ) ) ;
#1737 = VECTOR ( 'NONE', #16486, 1000.000000000000227 ) ;
#1738 = DIRECTION ( 'NONE',  ( -0.9730401042858036753, 0.2306359803922031493, 5.432877459303543355E-17 ) ) ;
#1739 = VERTEX_POINT ( 'NONE', #21751 ) ;
#1740 = CARTESIAN_POINT ( 'NONE',  ( -26.99999999999959854, -31.09999999999999787, -21.50000000000000000 ) ) ;
#1741 = ORIENTED_EDGE ( 'NONE', *, *, #10031, .F. ) ;
#1742 = CARTESIAN_POINT ( 'NONE',  ( 28.89837840081079889, -1.998294948772289858, -13.00000000000039968 ) ) ;
#1743 = CARTESIAN_POINT ( 'NONE',  ( -62.93704341833160498, 12.35813331950920002, 2.458500000000117147 ) ) ;
#1744 = CARTESIAN_POINT ( 'NONE',  ( 0.000000000000000000, 0.000000000000000000, -2.500000000000000000 ) ) ;
#1745 = VERTEX_POINT ( 'NONE', #22092 ) ;
#1746 = AXIS2_PLACEMENT_3D ( 'NONE', #2505, #18903, #22446 ) ;
#1747 = CIRCLE ( 'NONE', #22616, 5.000000000000001776 ) ;
#1748 = CARTESIAN_POINT ( 'NONE',  ( 0.03403376487640559500, -6.499910899608420500, -2.500000000000090150 ) ) ;
#1749 = DIRECTION ( 'NONE',  ( 0.9999862922474493931, 0.005235963827117055998, -1.750845403988397166E-31 ) ) ;
#1750 = VERTEX_POINT ( 'NONE', #130 ) ;
#1751 = APPLICATION_PROTOCOL_DEFINITION ( 'international standard', 'config_control_design', 1994, #19327 ) ;
#1752 = ORIENTED_EDGE ( 'NONE', *, *, #8865, .F. ) ;
#1753 = ORIENTED_EDGE ( 'NONE', *, *, #15494, .F. ) ;
#1754 = CARTESIAN_POINT ( 'NONE',  ( -23.50000000000000000, -20.00000000000000000, -2.500000000000000000 ) ) ;
#1755 = CALENDAR_DATE ( 2026, 31, 10 ) ;
#1756 = PLANE ( 'NONE',  #13502 ) ;
#1757 = CALENDAR_DATE ( 2026, 31, 10 ) ;
#1758 = DIRECTION ( 'NONE',  ( 0.000000000000000000, -1.000000000000000000, 9.355573283744330345E-16 ) ) ;
#1759 = VECTOR ( 'NONE', #19079, 1000.000000000000227 ) ;
#1760 = VECTOR ( 'NONE', #14465, 1000.000000000000000 ) ;
#1761 = VECTOR ( 'NONE', #2272, 1000.000000000000114 ) ;
#1762 = CARTESIAN_POINT ( 'NONE',  ( -26.75688440168130100, 6.359989102302520791, -2.500292893218799772 ) ) ;
#1763 = EDGE_CURVE ( 'NONE', #16953, #23364, #21851, .T. ) ;
#1764 = EDGE_CURVE ( 'NONE', #290, #6621, #7398, .T. ) ;
#1765 = PERSON_AND_ORGANIZATION ( #11966, #8758 ) ;
#1766 = ORIENTED_EDGE ( 'NONE', *, *, #7805, .T. ) ;
#1767 = DIRECTION ( 'NONE',  ( -8.911056267098788616E-18, -1.998401444326210262E-15, -1.000000000000000000 ) ) ;
#1768 = DIRECTION ( 'NONE',  ( 0.8511275218278948618, 0.5249589903860170104, -5.212440122911309516E-17 ) ) ;
#1769 = ORIENTED_EDGE ( 'NONE', *, *, #22920, .F. ) ;
#1770 = DIRECTION ( 'NONE',  ( 0.000000000000000000, 0.000000000000000000, -1.000000000000000000 ) ) ;
#1771 = LINE ( 'NONE', #15810, #14181 ) ;
#1772 = LINE ( 'NONE', #5576, #22850 ) ;
#1773 = AXIS2_PLACEMENT_3D ( 'NONE', #2635, #16883, #7865 ) ;
#1774 = ORIENTED_EDGE ( 'NONE', *, *, #14842, .F. ) ;
#1775 = VERTEX_POINT ( 'NONE', #22207 ) ;
#1776 = DIRECTION ( 'NONE',  ( 0.2306359803922085339, 0.9730401042858022320, 0.000000000000000000 ) ) ;
#1777 = EDGE_LOOP ( 'NONE', ( #15987, #12154, #3454, #18818, #13999, #11383, #9608, #3929, #11992, #18480, #4171, #13920 ) ) ;
#1778 = ADVANCED_FACE ( 'NONE', ( #5595 ), #349, .T. ) ;
#1779 = EDGE_CURVE ( 'NONE', #22384, #22303, #6078, .T. ) ;
#1780 = APPLICATION_PROTOCOL_DEFINITION ( 'international standard', 'config_control_design', 1994, #156 ) ;
#1781 = VECTOR ( 'NONE', #21078, 1000.000000000000000 ) ;
#1782 = VERTEX_POINT ( 'NONE', #11327 ) ;
#1783 = VERTEX_POINT ( 'NONE', #7505 ) ;
#1784 = CARTESIAN_POINT ( 'NONE',  ( 34.40839383886530101, 23.41606575285529956, 9.720299461620768966 ) ) ;
#1785 = CIRCLE ( 'NONE', #13936, 4.750000000000001776 ) ;
#1786 = CARTESIAN_POINT ( 'NONE',  ( -27.00000000000000000, -28.60000000000000142, 21.50000000000000000 ) ) ;
#1787 = MECHANICAL_CONTEXT ( 'NONE', #12343, 'mechanical' ) ;
#1788 = FACE_OUTER_BOUND ( 'NONE', #12114, .T. ) ;
#1789 = CARTESIAN_POINT ( 'NONE',  ( 3.242007008979478005E-15, -33.09999999999999432, 25.00000000000000000 ) ) ;
#1790 = CIRCLE ( 'NONE', #15071, 2.066999999999999282 ) ;
#1791 = VECTOR ( 'NONE', #11198, 1000.000000000000000 ) ;
#1792 = ORIENTED_EDGE ( 'NONE', *, *, #7942, .F. ) ;
#1794 = CARTESIAN_POINT ( 'NONE',  ( 118.5310588935630136, -6.697506338400800452, -20.00000000000000000 ) ) ;
#1793 = AXIS2_PLACEMENT_3D ( 'NONE', #4710, #10539, #2816 ) ;
#1795 = EDGE_CURVE ( 'NONE', #7126, #13085, #21247, .T. ) ;
#1796 = PERSON_AND_ORGANIZATION_ROLE ( 'design_supplier' ) ;
#1797 = VECTOR ( 'NONE', #6698, 1000.000000000000000 ) ;
#1798 = AXIS2_PLACEMENT_3D ( 'NONE', #388, #4201, #22355 ) ;
#1799 = CYLINDRICAL_SURFACE ( 'NONE', #17458, 3.499999999999999556 ) ;
#1800 = DIRECTION ( 'NONE',  ( -0.2306359803922101992, -0.9730401042858018990, 4.616450158279816491E-15 ) ) ;
#1801 = APPROVAL ( #19535, 'UNSPECIFIED' ) ;
#1802 = FACE_OUTER_BOUND ( 'NONE', #17758, .T. ) ;
#1803 = CARTESIAN_POINT ( 'NONE',  ( -19.99999999999819877, -20.00000000000000000, 8.000000000004540368 ) ) ;
#1804 = CC_DESIGN_DATE_AND_TIME_ASSIGNMENT ( #12626, #10968, ( #15633 ) ) ;
#1805 = CARTESIAN_POINT ( 'NONE',  ( 35.59419854219520118, 9.774809681453358934, -10.50000000000050093 ) ) ;
#1806 = ORIENTED_EDGE ( 'NONE', *, *, #10576, .F. ) ;
#1807 = CIRCLE ( 'NONE', #21522, 0.3999999999999998557 ) ;
#1808 = CARTESIAN_POINT ( 'NONE',  ( 34.73651500123170166, 11.67452289462551285, 8.849422422067890537 ) ) ;
#1809 = UNCERTAINTY_MEASURE_WITH_UNIT (LENGTH_MEASURE( 1.000000000000000082E-05 ), #16931, 'distance_accuracy_value', 'NONE');
#1810 = EDGE_CURVE ( 'NONE', #11102, #23420, #2675, .T. ) ;
#1811 = EDGE_CURVE ( 'NONE', #3857, #7119, #20440, .T. ) ;
#1812 = EDGE_LOOP ( 'NONE', ( #6178, #4530 ) ) ;
#1813 = DIRECTION ( 'NONE',  ( -0.8823529412199823119, 0.4705882352125332901, 1.992040791580033901E-13 ) ) ;
#1814 = DIRECTION ( 'NONE',  ( 5.791496838535410422E-15, 2.469238035320170149E-14, -1.000000000000000000 ) ) ;
#1815 = VECTOR ( 'NONE', #932, 1000.000000000000114 ) ;
#1816 = ORIENTED_EDGE ( 'NONE', *, *, #16620, .T. ) ;
#1817 = PLANE ( 'NONE',  #20611 ) ;
#1818 = ORIENTED_EDGE ( 'NONE', *, *, #13921, .T. ) ;
#1819 = CARTESIAN_POINT ( 'NONE',  ( 34.89491389100810181, 23.30074776265909975, -13.00000000000049916 ) ) ;
#1820 = AXIS2_PLACEMENT_3D ( 'NONE', #21514, #10622, #7054 ) ;
#1821 = DATE_TIME_ROLE ( 'classification_date' ) ;
#1822 = CARTESIAN_POINT ( 'NONE',  ( 53.20239347634441884, 27.69690417850089759, -2.499999999999986233 ) ) ;
#1823 = SHAPE_REPRESENTATION_RELATIONSHIP ( 'NONE' , 'NONE' ,  #9451, #22100 ) ;
#1824 = APPLICATION_CONTEXT ( 'configuration controlled 3d designs of mechanical parts and assemblies' ) ;
#1825 = CARTESIAN_POINT ( 'NONE',  ( 34.40839383886520153, 23.41606575285519654, -13.00000000000049916 ) ) ;
#1826 = CARTESIAN_POINT ( 'NONE',  ( 35.94015251278350576, 11.23436983788199761, -27.55602540378494325 ) ) ;
#1827 = EDGE_CURVE ( 'NONE', #7573, #5643, #23134, .T. ) ;
#1828 = APPROVAL_DATE_TIME ( #18113, #21194 ) ;
#1829 = LINE ( 'NONE', #21897, #15707 ) ;
#1830 = LINE ( 'NONE', #14662, #10546 ) ;
#1831 = DIRECTION ( 'NONE',  ( 0.002617981913558435191, -0.4999931461237237529, -0.8660254037844391517 ) ) ;
#1832 = DESIGN_CONTEXT ( 'detailed design', #5484, 'design' ) ;
#1833 = DIRECTION ( 'NONE',  ( -3.099353312215989243E-62, -1.872670541876879671E-92, 1.000000000000000000 ) ) ;
#1834 = CIRCLE ( 'NONE', #20814, 2.500999999999919954 ) ;
#1835 = CARTESIAN_POINT ( 'NONE',  ( 35.59419854219520118, 9.774809681453278998, -26.88000000000049994 ) ) ;
#1836 = DIRECTION ( 'NONE',  ( -0.9730401042858036753, 0.2306359803922028995, 5.959266323858677443E-17 ) ) ;
#1837 = EDGE_CURVE ( 'NONE', #18371, #8755, #756, .T. ) ;
#1839 = ORIENTED_EDGE ( 'NONE', *, *, #15220, .T. ) ;
#1838 = ADVANCED_FACE ( 'NONE', ( #4639 ), #4517, .F. ) ;
#1840 = ORIENTED_EDGE ( 'NONE', *, *, #16144, .T. ) ;
#1841 = LINE ( 'NONE', #5290, #17933 ) ;
#1842 = DIRECTION ( 'NONE',  ( -0.1997366180463769070, -0.8426774492125652660, 0.5000000000000002220 ) ) ;
#1843 = ORIENTED_EDGE ( 'NONE', *, *, #16910, .T. ) ;
#1844 = PERSON_AND_ORGANIZATION_ROLE ( 'creator' ) ;
#1845 = DIRECTION ( 'NONE',  ( 0.000000000000000000, -1.000000000000000000, 0.000000000000000000 ) ) ;
#1846 = VERTEX_POINT ( 'NONE', #9768 ) ;
#1847 = CARTESIAN_POINT ( 'NONE',  ( -0.03403376487617929685, 6.499910899608420500, 8.874490886070419291E-14 ) ) ;
#1848 = PERSON_AND_ORGANIZATION ( #11966, #8758 ) ;
#1849 = CALENDAR_DATE ( 2026, 31, 10 ) ;
#1850 = PLANE ( 'NONE',  #23330 ) ;
#1851 = MANIFOLD_SOLID_BREP ( 'Imported1', #316 ) ;
#1852 = EDGE_CURVE ( 'NONE', #15219, #8168, #14582, .T. ) ;
#1853 = LINE ( 'NONE', #7565, #21750 ) ;
#1854 = AXIS2_PLACEMENT_3D ( 'NONE', #12756, #14760, #17994 ) ;
#1855 = ORIENTED_EDGE ( 'NONE', *, *, #8239, .T. ) ;
#1856 = CYLINDRICAL_SURFACE ( 'NONE', #21887, 2.500000000000000000 ) ;
#1857 = EDGE_CURVE ( 'NONE', #21726, #9676, #5540, .T. ) ;
#1858 = ORIENTED_EDGE ( 'NONE', *, *, #5758, .F. ) ;
#1859 = DIRECTION ( 'NONE',  ( 0.000000000000000000, 0.000000000000000000, -1.000000000000000000 ) ) ;
#1860 = DIRECTION ( 'NONE',  ( -0.2306359803922028995, -0.9730401042858035643, -1.064172857958375654E-32 ) ) ;
#1861 = DIRECTION ( 'NONE',  ( -1.000000000000000000, -6.662111140531837817E-09, 1.110223024625157172E-14 ) ) ;
#1862 = ORIENTED_EDGE ( 'NONE', *, *, #4041, .F. ) ;
#1863 = EDGE_CURVE ( 'NONE', #2098, #22438, #8594, .T. ) ;
#1864 = COORDINATED_UNIVERSAL_TIME_OFFSET ( 0, 0, .AHEAD. ) ;
#1865 = ADVANCED_FACE ( 'NONE', ( #18905 ), #18840, .F. ) ;
#1866 = DIRECTION ( 'NONE',  ( 0.000000000000000000, 0.000000000000000000, -1.000000000000000000 ) ) ;
#1867 = APPLICATION_CONTEXT ( 'configuration controlled 3d designs of mechanical parts and assemblies' ) ;
#1868 = ORIENTED_EDGE ( 'NONE', *, *, #3956, .T. ) ;
#1869 = DATE_AND_TIME ( #7466, #15966 ) ;
#1870 = ORIENTED_EDGE ( 'NONE', *, *, #17946, .T. ) ;
#1871 = ORIENTED_EDGE ( 'NONE', *, *, #1641, .F. ) ;
#1872 = DIRECTION ( 'NONE',  ( 0.000000000000000000, -1.000000000000000000, -1.734723475976808278E-15 ) ) ;
#1873 = CARTESIAN_POINT ( 'NONE',  ( -57.16525610687759951, 12.70085888708699962, 5.715859474400029324E-15 ) ) ;
#1874 = APPROVAL_ROLE ( '' ) ;
#1875 = CIRCLE ( 'NONE', #15147, 4.000000000000000000 ) ;
#1876 = DIRECTION ( 'NONE',  ( 0.2306359803922080898, 0.9730401042858024541, -2.572202231434325988E-16 ) ) ;
#1877 = APPROVAL_STATUS ( 'not_yet_approved' ) ;
#1878 = DIRECTION ( 'NONE',  ( -2.829953705592110306E-16, -9.355573283744330345E-16, -1.000000000000000000 ) ) ;
#1879 = CIRCLE ( 'NONE', #4929, 12.49999999999999467 ) ;
#1880 = CARTESIAN_POINT ( 'NONE',  ( 45.07211867146820339, 28.08243186520834911, -20.00000000000029843 ) ) ;
#1881 = APPROVAL ( #16543, 'UNSPECIFIED' ) ;
#1882 = CALENDAR_DATE ( 2026, 31, 10 ) ;
#1883 = PRODUCT ( '1602p_c_25', '1602p_c_25', '', ( #13536 ) ) ;
#1884 = APPROVAL_PERSON_ORGANIZATION ( #11058, #15773, #21943 ) ;
#1885 = ORIENTED_EDGE ( 'NONE', *, *, #9372, .F. ) ;
#1886 = AXIS2_PLACEMENT_3D ( 'NONE', #1819, #4928, #19419 ) ;
#1887 = AXIS2_PLACEMENT_3D ( 'NONE', #13663, #22796, #11677 ) ;
#1888 = DIRECTION ( 'NONE',  ( -0.9997651245102160411, -0.02167246670483411256, 0.000000000000000000 ) ) ;
#1889 = VERTEX_POINT ( 'NONE', #4406 ) ;
#1890 = CARTESIAN_POINT ( 'NONE',  ( 5.000000000000000000, -28.60000000000000142, 6.250000000000000000 ) ) ;
#1891 = FACE_OUTER_BOUND ( 'NONE', #16050, .T. ) ;
#1892 = DIRECTION ( 'NONE',  ( -0.9999862922474492821, -0.005235963827121953122, 1.187304881134294758E-16 ) ) ;
#1893 = ORIENTED_EDGE ( 'NONE', *, *, #9719, .F. ) ;
#1894 = ORIENTED_EDGE ( 'NONE', *, *, #9526, .T. ) ;
#1895 = DIRECTION ( 'NONE',  ( -0.9730401042858024541, 0.2306359803922080898, 5.959266323858942451E-17 ) ) ;
#1896 = ORIENTED_EDGE ( 'NONE', *, *, #5171, .F. ) ;
#1897 = AXIS2_PLACEMENT_3D ( 'NONE', #18802, #21976, #20446 ) ;
#1898 = COORDINATED_UNIVERSAL_TIME_OFFSET ( 0, 0, .AHEAD. ) ;
#1899 = VERTEX_POINT ( 'NONE', #2745 ) ;
#1900 = ORIENTED_EDGE ( 'NONE', *, *, #20362, .F. ) ;
#1901 = CARTESIAN_POINT ( 'NONE',  ( 36.79228697538940196, -6.849707878650510118, -3.000000000000000000 ) ) ;
#1902 = AXIS2_PLACEMENT_3D ( 'NONE', #1557, #14166, #21405 ) ;
#1903 = CARTESIAN_POINT ( 'NONE',  ( 59.82545934899435025, -8.814969416697280735, 9.256279155971832418E-15 ) ) ;
#1904 = APPROVAL_STATUS ( 'not_yet_approved' ) ;
#1905 = PLANE ( 'NONE',  #10893 ) ;
#1906 = EDGE_CURVE ( 'NONE', #9182, #5106, #15792, .T. ) ;
#1907 = APPROVAL_PERSON_ORGANIZATION ( #4423, #8675, #22339 ) ;
#1908 = CARTESIAN_POINT ( 'NONE',  ( 35.59419854219520118, 9.774809681453469068, 10.50000000000020073 ) ) ;
#1909 =( NAMED_UNIT ( * ) PLANE_ANGLE_UNIT ( ) SI_UNIT ( $, .RADIAN. ) );
#1910 = AXIS2_PLACEMENT_3D ( 'NONE', #6136, #20855, #6018 ) ;
#1911 = VERTEX_POINT ( 'NONE', #19145 ) ;
#1912 = DIRECTION ( 'NONE',  ( -3.099353312215988811E-62, 1.001855809244433740E-92, 1.000000000000000000 ) ) ;
#1913 = PERSON_AND_ORGANIZATION ( #11966, #8758 ) ;
#1914 = ORIENTED_EDGE ( 'NONE', *, *, #1282, .T. ) ;
#1915 = DIRECTION ( 'NONE',  ( -0.005235963827108352890, 0.9999862922474493931, 5.936218956694023463E-19 ) ) ;
#1916 = DIRECTION ( 'NONE',  ( 6.123237831918399306E-17, -1.569224110909209817E-30, -1.000000000000000000 ) ) ;
#1917 = CLOSED_SHELL ( 'NONE', ( #2769, #13548, #5082, #6507, #15599, #11687, #1539, #685, #12602, #19975, #129, #4126, #23045, #6384, #3776, #21888, #21015, #21119, #12737, #7471, #15663, #22262, #1012 ) ) ;
#1918 = CARTESIAN_POINT ( 'NONE',  ( 36.09092202081949807, 8.115512906978191054, -27.69000000000049866 ) ) ;
#1919 = LOCAL_TIME ( 14, 11, 27.00000000000000000, #10471 ) ;
#1920 = CARTESIAN_POINT ( 'NONE',  ( 35.59419854219520118, 9.774809681453540122, 26.30000000000000071 ) ) ;
#1921 = PLANE ( 'NONE',  #19801 ) ;
#1922 = APPROVAL_PERSON_ORGANIZATION ( #2136, #211, #4510 ) ;
#1923 = ORIENTED_EDGE ( 'NONE', *, *, #8571, .F. ) ;
#1924 = CARTESIAN_POINT ( 'NONE',  ( 33.76470586405379493, 8.803418887774272505, 8.896078739569134086 ) ) ;
#1925 = ORIENTED_EDGE ( 'NONE', *, *, #22676, .F. ) ;
#1926 = PLANE ( 'NONE',  #6182 ) ;
#1927 = CARTESIAN_POINT ( 'NONE',  ( -62.94391562085439773, 13.67061532808409829, -5.515300856952130332E-15 ) ) ;
#1928 = SECURITY_CLASSIFICATION ( '', '', #15173 ) ;
#1929 = ORIENTED_EDGE ( 'NONE', *, *, #17674, .T. ) ;
#1930 = VECTOR ( 'NONE', #23331, 1000.000000000000000 ) ;
#1931 = DIRECTION ( 'NONE',  ( 3.764133351409869857E-47, -1.000000000000000000, 4.861311874385510251E-15 ) ) ;
#1932 = ADVANCED_FACE ( 'NONE', ( #9878 ), #11569, .T. ) ;
#1933 = MANIFOLD_SOLID_BREP ( 'Imported1', #14367 ) ;
#1934 = VERTEX_POINT ( 'NONE', #20554 ) ;
#1935 = DIRECTION ( 'NONE',  ( -0.9730401042858036753, 0.2306359803922031493, -2.740969466505752002E-16 ) ) ;
#1936 = COORDINATED_UNIVERSAL_TIME_OFFSET ( 0, 0, .AHEAD. ) ;
#1937 = CARTESIAN_POINT ( 'NONE',  ( 3.499952022866072543, 0.01832587339492582068, 8.822666031689207903E-14 ) ) ;
#1938 = CC_DESIGN_DATE_AND_TIME_ASSIGNMENT ( #16342, #12687, ( #22797 ) ) ;
#1939 = LOCAL_TIME ( 14, 11, 27.00000000000000000, #12557 ) ;
#1940 = SHAPE_REPRESENTATION_RELATIONSHIP ( 'NONE' , 'NONE' ,  #9313, #17587 ) ;
#1941 = LOCAL_TIME ( 14, 11, 27.00000000000000000, #7982 ) ;
#1942 = CIRCLE ( 'NONE', #11476, 2.500000000000001332 ) ;
#1943 = CYLINDRICAL_SURFACE ( 'NONE', #8490, 6.499999999999998224 ) ;
#1944 = EDGE_CURVE ( 'NONE', #16249, #21214, #7449, .T. ) ;
#1945 = EDGE_CURVE ( 'NONE', #17998, #6181, #708, .T. ) ;
#1946 = DIRECTION ( 'NONE',  ( -0.9730401042858024541, 0.2306359803922080898, 5.959266323858942451E-17 ) ) ;
#1947 = DIRECTION ( 'NONE',  ( 0.000000000000000000, 0.000000000000000000, 1.000000000000000000 ) ) ;
#1948 = AXIS2_PLACEMENT_3D ( 'NONE', #15826, #23055, #18078 ) ;
#1949 = CARTESIAN_POINT ( 'NONE',  ( 35.59419854219520118, 9.774809681453518806, 20.00000000000000000 ) ) ;
#1950 = CARTESIAN_POINT ( 'NONE',  ( 102.8131131701580046, 7.202356331284519797, 13.00000000000000000 ) ) ;
#1951 = DIRECTION ( 'NONE',  ( -1.138590270679734009E-14, -2.220446049251240387E-15, -1.000000000000000000 ) ) ;
#1952 = DIRECTION ( 'NONE',  ( -1.187319687680494078E-16, -2.805478249478255076E-20, -1.000000000000000000 ) ) ;
#1953 = DIRECTION ( 'NONE',  ( 0.000000000000000000, 0.000000000000000000, -1.000000000000000000 ) ) ;
#1954 = LINE ( 'NONE', #12886, #4264 ) ;
#1955 = ORIENTED_EDGE ( 'NONE', *, *, #13990, .T. ) ;
#1956 = LOCAL_TIME ( 14, 11, 27.00000000000000000, #8589 ) ;
#1957 = VERTEX_POINT ( 'NONE', #825 ) ;
#1958 = CARTESIAN_POINT ( 'NONE',  ( 39.27359436029389883, 22.26288585089439920, 12.99999999999970157 ) ) ;
#1959 = DIRECTION ( 'NONE',  ( -6.281952996264290168E-17, -4.969341027148640384E-15, -1.000000000000000000 ) ) ;
#1960 = ORIENTED_EDGE ( 'NONE', *, *, #6381, .T. ) ;
#1961 = AXIS2_PLACEMENT_3D ( 'NONE', #6347, #16468, #1860 ) ;
#1962 = CARTESIAN_POINT ( 'NONE',  ( -30.72441677844210162, -6.660963241697119841, 2.999000000000090260 ) ) ;
#1963 = EDGE_CURVE ( 'NONE', #15512, #7019, #10502, .T. ) ;
#1964 = ORIENTED_EDGE ( 'NONE', *, *, #8474, .F. ) ;
#1965 = DIRECTION ( 'NONE',  ( 0.000000000000000000, 0.000000000000000000, -1.000000000000000000 ) ) ;
#1966 = SECURITY_CLASSIFICATION ( '', '', #13605 ) ;
#1967 = PERSON_AND_ORGANIZATION ( #11966, #8758 ) ;
#1968 = CARTESIAN_POINT ( 'NONE',  ( 36.56362820255242241, 7.944277063050280141, -8.864716985163925145 ) ) ;
#1969 = CC_DESIGN_DATE_AND_TIME_ASSIGNMENT ( #20785, #4046, ( #13165 ) ) ;
#1970 = CC_DESIGN_PERSON_AND_ORGANIZATION_ASSIGNMENT ( #14727, #21958, ( #12523 ) ) ;
#1971 = CALENDAR_DATE ( 2026, 31, 10 ) ;
#1972 = AXIS2_PLACEMENT_3D ( 'NONE', #15325, #13438, #2385 ) ;
#1973 = DIRECTION ( 'NONE',  ( -1.000000000000000000, 0.000000000000000000, 0.000000000000000000 ) ) ;
#1974 = ADVANCED_FACE ( 'NONE', ( #15208 ), #10013, .F. ) ;
#1975 = ADVANCED_FACE ( 'NONE', ( #8098 ), #17352, .T. ) ;
#1976 = EDGE_LOOP ( 'NONE', ( #8688, #16014, #13668, #9572 ) ) ;
#1977 = APPROVAL_PERSON_ORGANIZATION ( #18163, #2995, #12593 ) ;
#1978 = PRODUCT_DEFINITION ( 'UNKNOWN', '', #16680, #4712 ) ;
#1979 = CARTESIAN_POINT ( 'NONE',  ( -25.64161990512560152, 6.365892616704879714, 5.000000000000000000 ) ) ;
#1980 = EDGE_CURVE ( 'NONE', #12251, #20636, #6307, .T. ) ;
#1981 = VERTEX_POINT ( 'NONE', #11786 ) ;
#1982 = CARTESIAN_POINT ( 'NONE',  ( -20.00000000397360012, 22.95208919256889857, -5.000000000000000000 ) ) ;
#1983 = AXIS2_PLACEMENT_3D ( 'NONE', #8504, #15732, #1343 ) ;
#1984 = VECTOR ( 'NONE', #1141, 1000.000000000000114 ) ;
#1985 = ORIENTED_EDGE ( 'NONE', *, *, #3441, .F. ) ;
#1986 = CARTESIAN_POINT ( 'NONE',  ( 36.84099409957980242, 22.83947580187480142, 13.00000000000000000 ) ) ;
#1987 = CARTESIAN_POINT ( 'NONE',  ( 89.62416413250210212, 10.32848256004259824, 12.99999999999970157 ) ) ;
#1988 = CARTESIAN_POINT ( 'NONE',  ( -20.00000000397270128, 22.95208919257349933, 8.000000000004460432 ) ) ;
#1989 = ORIENTED_EDGE ( 'NONE', *, *, #12764, .T. ) ;
#1990 = CIRCLE ( 'NONE', #6931, 2.499999999999998224 ) ;
#1991 = PERSON_AND_ORGANIZATION ( #22642, #20185 ) ;
#1992 = DIRECTION ( 'NONE',  ( 0.005235963827101452160, -0.9999862922474493931, 5.479105319409471602E-16 ) ) ;
#1993 = CIRCLE ( 'NONE', #23234, 2.066999999999999726 ) ;
#1994 = ORIENTED_EDGE ( 'NONE', *, *, #6302, .F. ) ;
#1995 = COORDINATED_UNIVERSAL_TIME_OFFSET ( 0, 0, .AHEAD. ) ;
#1996 = ADVANCED_FACE ( 'NONE', ( #17244 ), #946, .F. ) ;
#1997 = PRODUCT_DEFINITION_FORMATION_WITH_SPECIFIED_SOURCE ( 'ANY', '', #18416, .NOT_KNOWN. ) ;
#1998 = ORIENTED_EDGE ( 'NONE', *, *, #6028, .F. ) ;
#1999 = VERTEX_POINT ( 'NONE', #13661 ) ;
#2000 = DIRECTION ( 'NONE',  ( -0.2306359803922028717, -0.9730401042858034533, -4.546664459266603656E-32 ) ) ;
#2001 = CALENDAR_DATE ( 2026, 31, 10 ) ;
#2002 = AXIS2_PLACEMENT_3D ( 'NONE', #20195, #3925, #22310 ) ;
#2003 = AXIS2_PLACEMENT_3D ( 'NONE', #8609, #15845, #21425 ) ;
#2004 = PERSON ( 'NAUO-PER6', 'UNSPECIFIED', 'UNSPECIFIED', ('UNSPECIFIED'), ('UNSPECIFIED'), ('UNSPECIFIED') ) ;
#2005 = EDGE_CURVE ( 'NONE', #6113, #4832, #20901, .T. ) ;
#2006 = AXIS2_PLACEMENT_3D ( 'NONE', #17289, #15136, #20616 ) ;
#2007 = FACE_OUTER_BOUND ( 'NONE', #20434, .T. ) ;
#2008 = CALENDAR_DATE ( 2026, 31, 10 ) ;
#2009 = DIRECTION ( 'NONE',  ( 0.1630842657209384816, 0.6880432561069583786, -0.7071067811865453523 ) ) ;
#2010 = ADVANCED_FACE ( 'NONE', ( #3087 ), #23028, .T. ) ;
#2011 = ADVANCED_FACE ( 'NONE', ( #19360 ), #10357, .T. ) ;
#2012 =( LENGTH_UNIT ( ) NAMED_UNIT ( * ) SI_UNIT ( .MILLI., .METRE. ) );
#2014 = AXIS2_PLACEMENT_3D ( 'NONE', #8864, #12766, #1714 ) ;
#2013 = CARTESIAN_POINT ( 'NONE',  ( -22.52506283708579815, 28.95208917575130414, 6.750000000004479972 ) ) ;
#2015 = AXIS2_PLACEMENT_3D ( 'NONE', #10570, #17437, #21462 ) ;
#2016 = MECHANICAL_CONTEXT ( 'NONE', #5034, 'mechanical' ) ;
#2017 = LOCAL_TIME ( 14, 11, 27.00000000000000000, #540 ) ;
#2018 = VERTEX_POINT ( 'NONE', #5219 ) ;
#2019 = DIRECTION ( 'NONE',  ( 0.000000000000000000, 0.5102823824563427202, -0.8600069128528436968 ) ) ;
#2020 = ORIENTED_EDGE ( 'NONE', *, *, #3611, .T. ) ;
#2021 = CIRCLE ( 'NONE', #19477, 5.999999999999999112 ) ;
#2022 = MANIFOLD_SOLID_BREP ( 'Boss-Extrude1', #1917 ) ;
#2023 = CARTESIAN_POINT ( 'NONE',  ( -65.62876257020761273, -24.89748912807110059, 5.000000000000000000 ) ) ;
#2024 = AXIS2_PLACEMENT_3D ( 'NONE', #6807, #15715, #6696 ) ;
#2025 = DIRECTION ( 'NONE',  ( 6.123230199561429643E-17, 4.868008300101910084E-15, 1.000000000000000000 ) ) ;
#2026 = SHAPE_REPRESENTATION ( 'F2', ( #12739 ), #2093 ) ;
#2027 = CARTESIAN_POINT ( 'NONE',  ( 6.500000000000000000, -17.30000000000000071, 2.500000000000000000 ) ) ;
#2028 = VERTEX_POINT ( 'NONE', #21590 ) ;
#2029 = VERTEX_POINT ( 'NONE', #2970 ) ;
#2030 = LINE ( 'NONE', #16157, #7584 ) ;
#2031 = VERTEX_POINT ( 'NONE', #3320 ) ;
#2032 = APPLICATION_PROTOCOL_DEFINITION ( 'international standard', 'config_control_design', 1994, #15501 ) ;
#2033 = ORIENTED_EDGE ( 'NONE', *, *, #619, .T. ) ;
#2034 = ORIENTED_EDGE ( 'NONE', *, *, #6517, .F. ) ;
#2035 = DIRECTION ( 'NONE',  ( -0.9730401042858036753, 0.2306359803922031493, -2.804983810440356829E-16 ) ) ;
#2036 = VECTOR ( 'NONE', #21744, 1000.000000000000000 ) ;
#2037 = DIRECTION ( 'NONE',  ( 1.000000000000000000, -1.922967408714619726E-16, 0.000000000000000000 ) ) ;
#2038 = COORDINATED_UNIVERSAL_TIME_OFFSET ( 0, 0, .AHEAD. ) ;
#2039 = CARTESIAN_POINT ( 'NONE',  ( -19.55420733641118147, 2.397309549614596857, 4.999999999999993783 ) ) ;
#2040 = DIRECTION ( 'NONE',  ( 0.000000000000000000, 0.000000000000000000, -1.000000000000000000 ) ) ;
#2041 = ORIENTED_EDGE ( 'NONE', *, *, #19548, .F. ) ;
#2042 = DIRECTION ( 'NONE',  ( -0.9730401042858035643, 0.2306359803922028717, 5.958148513035547083E-17 ) ) ;
#2043 = DATE_TIME_ROLE ( 'creation_date' ) ;
#2044 = VERTEX_POINT ( 'NONE', #12257 ) ;
#2045 = DIRECTION ( 'NONE',  ( -4.028143194477080210E-16, -2.054129435991050111E-15, -1.000000000000000000 ) ) ;
#2046 = CARTESIAN_POINT ( 'NONE',  ( 42.82341786264429828, 18.59529084842182556, -13.00000000000029665 ) ) ;
#2047 = LINE ( 'NONE', #23181, #986 ) ;
#2048 = ADVANCED_FACE ( 'NONE', ( #1176 ), #12477, .T. ) ;
#2049 = VECTOR ( 'NONE', #9440, 1000.000000000000000 ) ;
#2050 = DIRECTION ( 'NONE',  ( -2.269700743865584947E-13, -2.220446049247695246E-15, -1.000000000000000000 ) ) ;
#2051 = CARTESIAN_POINT ( 'NONE',  ( 37.27955344062029752, 9.375336445360789028, 29.25000000000000000 ) ) ;
#2052 = ORIENTED_EDGE ( 'NONE', *, *, #9969, .T. ) ;
#2053 = AXIS2_PLACEMENT_3D ( 'NONE', #16011, #21699, #2221 ) ;
#2054 = CARTESIAN_POINT ( 'NONE',  ( 34.85451023951635108, 7.825865074983275882, 8.759424124906640685 ) ) ;
#2055 = EDGE_LOOP ( 'NONE', ( #14801, #2410 ) ) ;
#2056 = ORIENTED_EDGE ( 'NONE', *, *, #20372, .F. ) ;
#2057 = DIRECTION ( 'NONE',  ( -0.9999863470142587030, -0.005225493764090578461, -1.706795877867719251E-17 ) ) ;
#2058 = CARTESIAN_POINT ( 'NONE',  ( -20.00000000397270128, 22.95208919257159863, 5.500000000004459544 ) ) ;
#2059 = ORIENTED_EDGE ( 'NONE', *, *, #11244, .F. ) ;
#2060 = CARTESIAN_POINT ( 'NONE',  ( 62.70840910389689782, 3.348031886875279639, 1.061114750357439988E-14 ) ) ;
#2061 = ORIENTED_EDGE ( 'NONE', *, *, #14467, .F. ) ;
#2062 = CYLINDRICAL_SURFACE ( 'NONE', #14308, 3.500000000000001332 ) ;
#2063 = COORDINATED_UNIVERSAL_TIME_OFFSET ( 0, 0, .AHEAD. ) ;
#2064 = PLANE ( 'NONE',  #18503 ) ;
#2065 = DIRECTION ( 'NONE',  ( 0.005235963827101446956, -0.9999862922474495042, 5.479105319409467658E-16 ) ) ;
#2066 = DIRECTION ( 'NONE',  ( -0.2306359803922080343, -0.9730401042858022320, 1.412237191019910313E-17 ) ) ;
#2067 = DATE_AND_TIME ( #18357, #9524 ) ;
#2068 = CARTESIAN_POINT ( 'NONE',  ( -27.50000000434419789, 26.95208919188010199, -6.749999999993870681 ) ) ;
#2069 = CARTESIAN_POINT ( 'NONE',  ( 5.000000000000000000, -28.60000000000000142, -21.50000000000000000 ) ) ;
#2070 = EDGE_CURVE ( 'NONE', #12472, #22197, #18058, .T. ) ;
#2071 = CYLINDRICAL_SURFACE ( 'NONE', #11630, 5.000000000000001776 ) ;
#2072 = EDGE_CURVE ( 'NONE', #4537, #3647, #21376, .T. ) ;
#2073 = CARTESIAN_POINT ( 'NONE',  ( 28.94448933012489888, 0.3641629059907759425, 13.00000000000019895 ) ) ;
#2074 = DIRECTION ( 'NONE',  ( -6.123230174520380038E-17, -4.962644601432250805E-15, -1.000000000000000000 ) ) ;
#2075 = DIRECTION ( 'NONE',  ( -0.9730401042858036753, 0.2306359803922031493, -2.740969466505752002E-16 ) ) ;
#2076 = ORIENTED_EDGE ( 'NONE', *, *, #20373, .F. ) ;
#2077 = AXIS2_PLACEMENT_3D ( 'NONE', #11052, #8481, #9264 ) ;
#2078 = EDGE_LOOP ( 'NONE', ( #19476, #6876, #3014, #406 ) ) ;
#2079 = DIRECTION ( 'NONE',  ( -2.977235988022388482E-185, 9.605990953944227443E-124, 1.000000000000000000 ) ) ;
#2080 = DIRECTION ( 'NONE',  ( -0.2306359803922028717, -0.9730401042858034533, 1.407521210652564497E-17 ) ) ;
#2081 = VERTEX_POINT ( 'NONE', #17594 ) ;
#2082 = EDGE_CURVE ( 'NONE', #7665, #6041, #6784, .T. ) ;
#2083 = EDGE_CURVE ( 'NONE', #12797, #6625, #598, .T. ) ;
#2084 = DIRECTION ( 'NONE',  ( 0.000000000000000000, 0.000000000000000000, 1.000000000000000000 ) ) ;
#2085 = EDGE_LOOP ( 'NONE', ( #16858, #59, #11665 ) ) ;
#2086 = CARTESIAN_POINT ( 'NONE',  ( -26.75688440168130100, 6.359989102302520791, 2.500292893218799772 ) ) ;
#2087 = MECHANICAL_CONTEXT ( 'NONE', #1824, 'mechanical' ) ;
#2088 = CARTESIAN_POINT ( 'NONE',  ( 37.61307566641299616, 10.23834044308586044, -8.954072598562484941 ) ) ;
#2089 = PRODUCT_DEFINITION_SHAPE ( 'NONE', 'NONE',  #23478 ) ;
#2090 = SECURITY_CLASSIFICATION_LEVEL ( 'unclassified' ) ;
#2091 = CARTESIAN_POINT ( 'NONE',  ( 2.500000000000000000, -31.09999999999999787, -19.00000000000000000 ) ) ;
#2092 = ORIENTED_EDGE ( 'NONE', *, *, #9406, .T. ) ;
#2093 =( GEOMETRIC_REPRESENTATION_CONTEXT ( 3 ) GLOBAL_UNCERTAINTY_ASSIGNED_CONTEXT ( ( #1809 ) ) GLOBAL_UNIT_ASSIGNED_CONTEXT ( ( #16931, #22154, #17045 ) ) REPRESENTATION_CONTEXT ( 'NONE', 'WORKASPACE' ) );
#2094 = CARTESIAN_POINT ( 'NONE',  ( 35.59419854219520118, 9.774809681453278998, -26.88000000000049994 ) ) ;
#2095 = ORIENTED_EDGE ( 'NONE', *, *, #14638, .T. ) ;
#2096 = CARTESIAN_POINT ( 'NONE',  ( 43.84419854219520118, 9.774809681453278998, 25.00000000000000000 ) ) ;
#2097 = EDGE_CURVE ( 'NONE', #15533, #4748, #9740, .T. ) ;
#2098 = VERTEX_POINT ( 'NONE', #10705 ) ;
#2099 = CYLINDRICAL_SURFACE ( 'NONE', #8210, 2.500000000000000000 ) ;
#2100 = DIRECTION ( 'NONE',  ( -1.187319687680494078E-16, -2.805478249478260493E-20, -1.000000000000000000 ) ) ;
#2101 = ORIENTED_EDGE ( 'NONE', *, *, #20735, .F. ) ;
#2102 = APPROVAL ( #758, 'UNSPECIFIED' ) ;
#2103 = DATE_AND_TIME ( #9356, #14111 ) ;
#2104 = CC_DESIGN_PERSON_AND_ORGANIZATION_ASSIGNMENT ( #11288, #2589, ( #19768 ) ) ;
#2105 = DIRECTION ( 'NONE',  ( 3.099353312215989243E-62, -1.534091707905539548E-92, -1.000000000000000000 ) ) ;
#2106 = EDGE_LOOP ( 'NONE', ( #2283, #19043, #9151, #21840 ) ) ;
#2107 = EDGE_CURVE ( 'NONE', #13193, #2417, #16139, .T. ) ;
#2108 = EDGE_CURVE ( 'NONE', #21983, #22720, #10113, .T. ) ;
#2109 = PERSON_AND_ORGANIZATION ( #11966, #8758 ) ;
#2110 = DIRECTION ( 'NONE',  ( 0.000000000000000000, 1.668003342285391304E-16, 1.000000000000000000 ) ) ;
#2111 = ORIENTED_EDGE ( 'NONE', *, *, #20825, .T. ) ;
#2112 = VERTEX_POINT ( 'NONE', #13899 ) ;
#2113 = EDGE_CURVE ( 'NONE', #8342, #16244, #14243, .T. ) ;
#2114 = DIRECTION ( 'NONE',  ( -0.9997648975362233292, -0.02168293463498000007, 0.000000000000000000 ) ) ;
#2115 = COORDINATED_UNIVERSAL_TIME_OFFSET ( 0, 0, .AHEAD. ) ;
#2116 = AXIS2_PLACEMENT_3D ( 'NONE', #22136, #20361, #22595 ) ;
#2117 = DIRECTION ( 'NONE',  ( 0.005235963827104182615, -0.9999862922474495042, -5.936218956636744380E-19 ) ) ;
#2118 = COORDINATED_UNIVERSAL_TIME_OFFSET ( 0, 0, .AHEAD. ) ;
#2119 = DIRECTION ( 'NONE',  ( 0.8660135325225010172, 0.004534477687572223414, -0.5000000000000000000 ) ) ;
#2120 = LINE ( 'NONE', #9376, #3895 ) ;
#2121 = APPLICATION_PROTOCOL_DEFINITION ( 'international standard', 'config_control_design', 1994, #5034 ) ;
#2122 = EDGE_CURVE ( 'NONE', #23060, #1637, #19708, .T. ) ;
#2123 = CIRCLE ( 'NONE', #4795, 2.500000000000000000 ) ;
#2124 = EDGE_LOOP ( 'NONE', ( #14350, #6851, #3150, #21931 ) ) ;
#2125 = DIRECTION ( 'NONE',  ( -4.526956032885830318E-15, -4.330888464475804873E-31, 1.000000000000000000 ) ) ;
#2126 = ORIENTED_EDGE ( 'NONE', *, *, #13290, .F. ) ;
#2127 = DIRECTION ( 'NONE',  ( 0.005235963827101446956, -0.9999862922474495042, 5.479105319409467658E-16 ) ) ;
#2128 = CARTESIAN_POINT ( 'NONE',  ( 35.59419854219520118, 9.774809681453550780, 26.88000000000000256 ) ) ;
#2129 = DIRECTION ( 'NONE',  ( 0.9730401042858035643, -0.2306359803922028717, 2.740969466505749044E-16 ) ) ;
#2130 = ORIENTED_EDGE ( 'NONE', *, *, #9185, .F. ) ;
#2131 = ORIENTED_EDGE ( 'NONE', *, *, #385, .F. ) ;
#2132 = DIRECTION ( 'NONE',  ( -1.000000000000000000, 0.000000000000000000, -3.099353312215991402E-62 ) ) ;
#2133 = ORIENTED_EDGE ( 'NONE', *, *, #10985, .T. ) ;
#2134 = EDGE_CURVE ( 'NONE', #9676, #5106, #1648, .T. ) ;
#2135 = EDGE_CURVE ( 'NONE', #22213, #9474, #3256, .T. ) ;
#2136 = PERSON_AND_ORGANIZATION ( #11966, #8758 ) ;
#2137 = ORIENTED_EDGE ( 'NONE', *, *, #10292, .F. ) ;
#2138 = ORIENTED_EDGE ( 'NONE', *, *, #1795, .T. ) ;
#2139 = DIRECTION ( 'NONE',  ( -0.9730401042858022320, 0.2306359803922080343, 5.959266323858941219E-17 ) ) ;
#2140 = CARTESIAN_POINT ( 'NONE',  ( 35.01760859121469593, 7.342209420739012060, 20.00000000000001066 ) ) ;
#2141 = APPROVAL_STATUS ( 'not_yet_approved' ) ;
#2142 = APPLICATION_CONTEXT ( 'configuration controlled 3d designs of mechanical parts and assemblies' ) ;
#2143 = DIRECTION ( 'NONE',  ( 6.123230174520409620E-17, 4.962644601432260272E-15, 1.000000000000000000 ) ) ;
#2144 = VECTOR ( 'NONE', #2623, 999.9999999999998863 ) ;
#2145 = DIRECTION ( 'NONE',  ( -0.2306359803922101437, -0.9730401042858017879, 4.316864774682981680E-15 ) ) ;
#2146 = CIRCLE ( 'NONE', #8228, 2.499999999999998668 ) ;
#2147 = AXIS2_PLACEMENT_3D ( 'NONE', #7748, #16634, #4176 ) ;
#2148 = SHAPE_REPRESENTATION_RELATIONSHIP ( 'NONE' , 'NONE' ,  #20817, #11367 ) ;
#2149 = ORIENTED_EDGE ( 'NONE', *, *, #12866, .T. ) ;
#2150 = DIRECTION ( 'NONE',  ( -0.5249589903860224505, 0.8511275218278915311, 1.187479569643817911E-16 ) ) ;
#2151 = DATE_TIME_ROLE ( 'classification_date' ) ;
#2152 = EDGE_CURVE ( 'NONE', #11903, #7064, #10865, .T. ) ;
#2153 = ORIENTED_EDGE ( 'NONE', *, *, #12007, .F. ) ;
#2154 = AXIS2_PLACEMENT_3D ( 'NONE', #1920, #7408, #9179 ) ;
#2155 = LINE ( 'NONE', #20565, #4947 ) ;
#2156 = FACE_OUTER_BOUND ( 'NONE', #8635, .T. ) ;
#2157 = CARTESIAN_POINT ( 'NONE',  ( 36.11419503630708050, 11.96864536137832324, 10.74538000000018911 ) ) ;
#2158 = VECTOR ( 'NONE', #19665, 1000.000000000000000 ) ;
#2159 = LINE ( 'NONE', #605, #5577 ) ;
#2160 = AXIS2_PLACEMENT_3D ( 'NONE', #7379, #8805, #17825 ) ;
#2161 = EDGE_CURVE ( 'NONE', #16704, #20682, #13131, .T. ) ;
#2162 = CYLINDRICAL_SURFACE ( 'NONE', #2377, 3.499999999999999556 ) ;
#2163 = ORIENTED_EDGE ( 'NONE', *, *, #3979, .F. ) ;
#2164 = FACE_BOUND ( 'NONE', #496, .T. ) ;
#2165 = ADVANCED_FACE ( 'NONE', ( #16397 ), #5155, .T. ) ;
#2167 = EDGE_CURVE ( 'NONE', #3931, #7660, #589, .T. ) ;
#2166 = ORIENTED_EDGE ( 'NONE', *, *, #11222, .F. ) ;
#2168 = ORIENTED_EDGE ( 'NONE', *, *, #6785, .T. ) ;
#2169 = DIRECTION ( 'NONE',  ( 0.8846153846153629319, -0.4663213712685850276, 0.000000000000000000 ) ) ;
#2170 = DIRECTION ( 'NONE',  ( 0.2306359803922031493, 0.9730401042858033422, -1.407521210652540462E-17 ) ) ;
#2171 = AXIS2_PLACEMENT_3D ( 'NONE', #14413, #19765, #12658 ) ;
#2172 = ORIENTED_EDGE ( 'NONE', *, *, #11346, .F. ) ;
#2173 = CARTESIAN_POINT ( 'NONE',  ( 117.1933702072879981, -12.34113894325840022, -19.59999999999999787 ) ) ;
#2174 = CARTESIAN_POINT ( 'NONE',  ( -19.99975861755300244, 22.95209442650120124, 3.749999999999900080 ) ) ;
#2175 = VECTOR ( 'NONE', #7146, 1000.000000000000000 ) ;
#2176 = ITEM_DEFINED_TRANSFORMATION ( 'NONE', 'NONE', #21252,  #12739 ) ;
#2177 = DIRECTION ( 'NONE',  ( -0.2306359803922066187, -0.9730401042858026761, 0.000000000000000000 ) ) ;
#2178 = VECTOR ( 'NONE', #6582, 999.9999999999998863 ) ;
#2179 = CIRCLE ( 'NONE', #18110, 4.250000000000000000 ) ;
#2180 = DIRECTION ( 'NONE',  ( -2.656137997592320068E-16, 6.783012436524469908E-17, 1.000000000000000000 ) ) ;
#2181 = DIRECTION ( 'NONE',  ( -2.065223582182029992E-34, 2.636263576915770120E-16, -1.000000000000000000 ) ) ;
#2182 = PERSON_AND_ORGANIZATION ( #11966, #8758 ) ;
#2183 = DIRECTION ( 'NONE',  ( -1.248400535696349791E-16, 3.446306084657144903E-17, 1.000000000000000000 ) ) ;
#2184 = CIRCLE ( 'NONE', #17378, 6.999999999999998224 ) ;
#2185 = DIRECTION ( 'NONE',  ( 0.9730401042858024541, -0.2306359803922080898, -5.959266323858942451E-17 ) ) ;
#2186 = APPROVAL ( #7515, 'UNSPECIFIED' ) ;
#2187 = DIRECTION ( 'NONE',  ( -2.269747459788994803E-13, -2.220446049250320181E-15, -1.000000000000000000 ) ) ;
#2188 = CARTESIAN_POINT ( 'NONE',  ( -16.50058068176721804, 23.02794805996685668, 4.999999999999900524 ) ) ;
#2189 = VECTOR ( 'NONE', #21948, 1000.000000000000000 ) ;
#2190 = CYLINDRICAL_SURFACE ( 'NONE', #878, 4.250000000000000000 ) ;
#2191 = LINE ( 'NONE', #18478, #22833 ) ;
#2192 = ORIENTED_EDGE ( 'NONE', *, *, #1319, .T. ) ;
#2193 = CIRCLE ( 'NONE', #10568, 2.500000000000000444 ) ;
#2194 = ORIENTED_EDGE ( 'NONE', *, *, #10217, .F. ) ;
#2195 = DIRECTION ( 'NONE',  ( -6.662161100567945949E-09, 1.000000000000000000, -2.081668171172169697E-15 ) ) ;
#2196 = VECTOR ( 'NONE', #14550, 1000.000000000000114 ) ;
#2197 = LINE ( 'NONE', #7438, #10653 ) ;
#2198 = ORIENTED_EDGE ( 'NONE', *, *, #9767, .T. ) ;
#2199 = LINE ( 'NONE', #5532, #9602 ) ;
#2200 = VERTEX_POINT ( 'NONE', #21828 ) ;
#2201 = CARTESIAN_POINT ( 'NONE',  ( 36.30836311812279860, 20.59233593730800038, 13.00000000000000000 ) ) ;
#2202 = PERSON_AND_ORGANIZATION ( #11966, #8758 ) ;
#2203 = CARTESIAN_POINT ( 'NONE',  ( -28.95596696049959817, -6.651703575491109355, -4.767474059747899950 ) ) ;
#2204 = ADVANCED_FACE ( 'NONE', ( #2007 ), #14481, .F. ) ;
#2205 = PERSON_AND_ORGANIZATION_ROLE ( 'classification_officer' ) ;
#2206 = AXIS2_PLACEMENT_3D ( 'NONE', #15624, #8522, #1003 ) ;
#2207 = CARTESIAN_POINT ( 'NONE',  ( -19.49999999982519938, -0.1021026942257859949, -3.750000000000000000 ) ) ;
#2208 = LINE ( 'NONE', #18494, #20789 ) ;
#2209 = VERTEX_POINT ( 'NONE', #22058 ) ;
#2210 = AXIS2_PLACEMENT_3D ( 'NONE', #14856, #22101, #13211 ) ;
#2211 = CARTESIAN_POINT ( 'NONE',  ( 28.54501609403219931, -1.321191992434360030, 11.00000000000019895 ) ) ;
#2212 = EDGE_LOOP ( 'NONE', ( #20429, #20832, #3918, #6569 ) ) ;
#2213 = CARTESIAN_POINT ( 'NONE',  ( 38.02679880290970260, 9.198219730473017108, 26.30000000000000426 ) ) ;
#2214 = ADVANCED_FACE ( 'NONE', ( #18409 ), #9135, .T. ) ;
#2215 = DIRECTION ( 'NONE',  ( 0.1997366180463769070, 0.8426774492125652660, 0.5000000000000003331 ) ) ;
#2216 = ORIENTED_EDGE ( 'NONE', *, *, #8255, .T. ) ;
#2217 = CARTESIAN_POINT ( 'NONE',  ( 37.13840842239409312, 23.31972727237329934, 15.00000000000000000 ) ) ;
#2218 = DIRECTION ( 'NONE',  ( 0.9822618273148069346, -0.1875145397033960160, 4.845439952583188648E-16 ) ) ;
#2219 = DIRECTION ( 'NONE',  ( -0.2306359803922080343, -0.9730401042858022320, 2.539064864905560527E-14 ) ) ;
#2220 = ORIENTED_EDGE ( 'NONE', *, *, #6488, .T. ) ;
#2221 = DIRECTION ( 'NONE',  ( -0.2306359803922030105, -0.9730401042858034533, 0.000000000000000000 ) ) ;
#2222 = ORIENTED_EDGE ( 'NONE', *, *, #17682, .T. ) ;
#2223 = PERSON_AND_ORGANIZATION_ROLE ( 'classification_officer' ) ;
#2224 = FACE_OUTER_BOUND ( 'NONE', #2124, .T. ) ;
#2225 = ORIENTED_EDGE ( 'NONE', *, *, #2852, .F. ) ;
#2226 = ORIENTED_EDGE ( 'NONE', *, *, #15706, .T. ) ;
#2227 = CLOSED_SHELL ( 'NONE', ( #11474, #18289, #19653, #15993, #3459, #2835 ) ) ;
#2228 = DIRECTION ( 'NONE',  ( -0.9730401042858036753, 0.2306359803922028995, 5.958148513035547083E-17 ) ) ;
#2229 = PERSON_AND_ORGANIZATION ( #11966, #8758 ) ;
#2230 = EDGE_CURVE ( 'NONE', #6743, #6798, #12017, .T. ) ;
#2231 = CARTESIAN_POINT ( 'NONE',  ( 35.59419854219520118, 9.774809681453278998, -25.00000000000000000 ) ) ;
#2232 = AXIS2_PLACEMENT_3D ( 'NONE', #15132, #22370, #6116 ) ;
#2233 = APPROVAL ( #9434, 'UNKNOWN' ) ;
#2234 = CARTESIAN_POINT ( 'NONE',  ( 37.01481097301073930, 22.79827665208023291, -11.00000000000049560 ) ) ;
#2235 = EDGE_CURVE ( 'NONE', #18419, #15816, #7076, .T. ) ;
#2236 = EDGE_CURVE ( 'NONE', #2850, #22077, #5561, .T. ) ;
#2237 = SECURITY_CLASSIFICATION_LEVEL ( 'unclassified' ) ;
#2238 = ORIENTED_EDGE ( 'NONE', *, *, #1906, .T. ) ;
#2239 = FACE_OUTER_BOUND ( 'NONE', #13971, .T. ) ;
#2240 = EDGE_LOOP ( 'NONE', ( #2333, #12408, #10818, #1955, #22375, #366 ) ) ;
#2241 = PERSON ( 'NAUO-PER13', 'UNSPECIFIED', 'UNSPECIFIED', ('UNSPECIFIED'), ('UNSPECIFIED'), ('UNSPECIFIED') ) ;
#2242 = DIRECTION ( 'NONE',  ( -0.9730401042858036753, 0.2306359803922031493, -2.740969466505752002E-16 ) ) ;
#2243 = DIRECTION ( 'NONE',  ( 2.874764335373299684E-17, -2.286959927910970108E-15, -1.000000000000000000 ) ) ;
#2244 = DIRECTION ( 'NONE',  ( 1.000000000000000000, -8.896220237034308570E-17, 0.000000000000000000 ) ) ;
#2245 = VERTEX_POINT ( 'NONE', #13063 ) ;
#2246 = CC_DESIGN_SECURITY_CLASSIFICATION ( #7962, ( #23483 ) ) ;
#2247 = EDGE_LOOP ( 'NONE', ( #15108, #11964, #12244, #10519 ) ) ;
#2249 = FACE_OUTER_BOUND ( 'NONE', #18547, .T. ) ;
#2248 = AXIS2_PLACEMENT_3D ( 'NONE', #5616, #21993, #12987 ) ;
#2250 = ORIENTED_EDGE ( 'NONE', *, *, #16123, .F. ) ;
#2251 = DATE_AND_TIME ( #11319, #17873 ) ;
#2252 = ORIENTED_EDGE ( 'NONE', *, *, #12127, .T. ) ;
#2253 = ORIENTED_EDGE ( 'NONE', *, *, #14709, .T. ) ;
#2254 = DIRECTION ( 'NONE',  ( -0.9730401042858022320, 0.2306359803922080343, 5.959266323858941219E-17 ) ) ;
#2255 = CYLINDRICAL_SURFACE ( 'NONE', #20918, 3.499999999999999556 ) ;
#2256 = APPROVAL_STATUS ( 'not_yet_approved' ) ;
#2257 = CARTESIAN_POINT ( 'NONE',  ( 36.68971944905815974, 14.39675017681084945, -27.87500000000052580 ) ) ;
#2258 = EDGE_CURVE ( 'NONE', #17265, #18737, #5331, .T. ) ;
#2259 = CARTESIAN_POINT ( 'NONE',  ( 37.46113131852554545, -4.027891576223090020, -13.00000000000000000 ) ) ;
#2260 = CC_DESIGN_DATE_AND_TIME_ASSIGNMENT ( #16711, #440, ( #6551 ) ) ;
#2261 = CC_DESIGN_PERSON_AND_ORGANIZATION_ASSIGNMENT ( #4160, #13083, ( #8957 ) ) ;
#2262 =( NAMED_UNIT ( * ) PLANE_ANGLE_UNIT ( ) SI_UNIT ( $, .RADIAN. ) );
#2263 = AXIS2_PLACEMENT_3D ( 'NONE', #11968, #2802, #15498 ) ;
#2264 =( GEOMETRIC_REPRESENTATION_CONTEXT ( 3 ) GLOBAL_UNCERTAINTY_ASSIGNED_CONTEXT ( ( #7928 ) ) GLOBAL_UNIT_ASSIGNED_CONTEXT ( ( #4646, #11789, #6547 ) ) REPRESENTATION_CONTEXT ( 'NONE', 'WORKASPACE' ) );
#2265 = ADVANCED_FACE ( 'NONE', ( #3664, #21714 ), #1756, .T. ) ;
#2266 = ADVANCED_FACE ( 'NONE', ( #12817 ), #18165, .T. ) ;
#2267 = ORIENTED_EDGE ( 'NONE', *, *, #5288, .F. ) ;
#2268 = CARTESIAN_POINT ( 'NONE',  ( -20.00000000000000000, -20.00000000000000000, 5.000000000000000000 ) ) ;
#2269 = PERSON_AND_ORGANIZATION ( #11966, #8758 ) ;
#2270 = ORIENTED_EDGE ( 'NONE', *, *, #22306, .T. ) ;
#2271 = CARTESIAN_POINT ( 'NONE',  ( -29.01753512594849838, 6.974156885510950588, 2.500000000000000000 ) ) ;
#2272 = DIRECTION ( 'NONE',  ( 0.2867834340965239592, -0.9579954394086668268, 4.742590440343770138E-15 ) ) ;
#2273 = VECTOR ( 'NONE', #5849, 1000.000000000000000 ) ;
#2274 = ORIENTED_EDGE ( 'NONE', *, *, #3323, .T. ) ;
#2275 = CARTESIAN_POINT ( 'NONE',  ( -26.99999999999959854, -19.33065833018799751, -21.50000000000000000 ) ) ;
#2276 = CARTESIAN_POINT ( 'NONE',  ( -60.04781580374580585, 11.89276268270289982, -5.000000000000000000 ) ) ;
#2277 = VERTEX_POINT ( 'NONE', #3562 ) ;
#2278 = DIRECTION ( 'NONE',  ( -0.9730401042858024541, 0.2306359803922080898, 5.959266323858942451E-17 ) ) ;
#2279 = DATE_AND_TIME ( #15107, #390 ) ;
#2280 = PRODUCT_DEFINITION_SHAPE ( 'NONE', 'NONE',  #23504 ) ;
#2281 = LOCAL_TIME ( 14, 11, 27.00000000000000000, #20304 ) ;
#2282 = ORIENTED_EDGE ( 'NONE', *, *, #13473, .T. ) ;
#2283 = ORIENTED_EDGE ( 'NONE', *, *, #21029, .T. ) ;
#2284 = CARTESIAN_POINT ( 'NONE',  ( 49.94654008041209892, 6.372928970669730298, 3.830789599272820115E-14 ) ) ;
#2285 = DIRECTION ( 'NONE',  ( -0.04564792618501069266, -0.9989575901083128651, 2.775557561562892534E-15 ) ) ;
#2286 =( GEOMETRIC_REPRESENTATION_CONTEXT ( 3 ) GLOBAL_UNCERTAINTY_ASSIGNED_CONTEXT ( ( #5857 ) ) GLOBAL_UNIT_ASSIGNED_CONTEXT ( ( #8867, #12878, #3729 ) ) REPRESENTATION_CONTEXT ( 'NONE', 'WORKASPACE' ) );
#2287 = VERTEX_POINT ( 'NONE', #9368 ) ;
#2288 = PERSON_AND_ORGANIZATION ( #11966, #8758 ) ;
#2289 = AXIS2_PLACEMENT_3D ( 'NONE', #23190, #15610, #19643 ) ;
#2290 = FACE_OUTER_BOUND ( 'NONE', #17184, .T. ) ;
#2291 = ADVANCED_FACE ( 'NONE', ( #11050 ), #13874, .F. ) ;
#2292 = DIRECTION ( 'NONE',  ( -1.000000000000000000, 0.000000000000000000, -3.099353312215989675E-62 ) ) ;
#2293 = PERSON_AND_ORGANIZATION ( #7107, #14552 ) ;
#2294 = CARTESIAN_POINT ( 'NONE',  ( -11.00000000000000000, -27.34999999999999787, -6.250000000000000000 ) ) ;
#2295 = AXIS2_PLACEMENT_3D ( 'NONE', #1064, #8454, #14021 ) ;
#2296 = PERSON ( 'NAUO-PER1', 'UNSPECIFIED', 'UNSPECIFIED', ('UNSPECIFIED'), ('UNSPECIFIED'), ('UNSPECIFIED') ) ;
#2297 =( BOUNDED_CURVE ( )  B_SPLINE_CURVE ( 2, ( #19632, #16412, #1918 ),
 .UNSPECIFIED., .F., .F. ) 
 B_SPLINE_CURVE_WITH_KNOTS ( ( 3, 3 ),
 ( 0.000000000000000000, 0.1752654207116860208 ),
 .UNSPECIFIED. ) 
 CURVE ( )  GEOMETRIC_REPRESENTATION_ITEM ( )  RATIONAL_B_SPLINE_CURVE ( ( 1.000000000000000000, 1.154700538379239916, 1.000000000000000000 ) ) 
 REPRESENTATION_ITEM ( '' )  );
#2298 = SHAPE_REPRESENTATION_RELATIONSHIP ( 'NONE' , 'NONE' ,  #7169, #18164 ) ;
#2299 = FACE_OUTER_BOUND ( 'NONE', #2078, .T. ) ;
#2300 = EDGE_CURVE ( 'NONE', #16709, #6326, #16594, .T. ) ;
#2301 = DIRECTION ( 'NONE',  ( 0.005235963827117091560, -0.9999862922474493931, -2.636227439666999735E-16 ) ) ;
#2302 = COORDINATED_UNIVERSAL_TIME_OFFSET ( 0, 0, .AHEAD. ) ;
#2303 = CC_DESIGN_APPROVAL ( #21286, ( #14615 ) ) ;
#2304 = EDGE_CURVE ( 'NONE', #16923, #18417, #15003, .T. ) ;
#2305 = APPROVAL_PERSON_ORGANIZATION ( #11871, #15029, #17428 ) ;
#2306 = DIRECTION ( 'NONE',  ( -1.320147222947483248E-46, 2.155962677239134989E-30, 1.000000000000000000 ) ) ;
#2308 = CARTESIAN_POINT ( 'NONE',  ( 39.94748832170330388, 24.67242251356951144, -13.00000000000049916 ) ) ;
#2307 = CONICAL_SURFACE ( 'NONE', #16003, 2.283500000000000529, 0.7853981633974419507 ) ;
#2309 = DIRECTION ( 'NONE',  ( 1.187319687680494078E-16, 2.805478249478255076E-20, 1.000000000000000000 ) ) ;
#2310 = CC_DESIGN_APPROVAL ( #3685, ( #17552 ) ) ;
#2311 = DIRECTION ( 'NONE',  ( -4.028143194477080210E-16, -2.054129435991050111E-15, -1.000000000000000000 ) ) ;
#2312 = PLANE ( 'NONE',  #17147 ) ;
#2313 = AXIS2_PLACEMENT_3D ( 'NONE', #14663, #20127, #16322 ) ;
#2314 = VERTEX_POINT ( 'NONE', #10897 ) ;
#2315 = ORIENTED_EDGE ( 'NONE', *, *, #15123, .F. ) ;
#2316 = DIRECTION ( 'NONE',  ( -0.9730401042858036753, 0.2306359803922028995, 5.958148513035547083E-17 ) ) ;
#2317 = FACE_OUTER_BOUND ( 'NONE', #17838, .T. ) ;
#2318 = EDGE_LOOP ( 'NONE', ( #12968, #6059, #17001 ) ) ;
#2319 = CARTESIAN_POINT ( 'NONE',  ( -32.65691263631629226, 9.274125246214079965, 5.000000000000000000 ) ) ;
#2320 = ORIENTED_EDGE ( 'NONE', *, *, #17834, .T. ) ;
#2321 = LOCAL_TIME ( 14, 11, 27.00000000000000000, #673 ) ;
#2322 = CARTESIAN_POINT ( 'NONE',  ( 117.1011158151309957, -12.73035498497280038, -20.00000000000000000 ) ) ;
#2323 = SECURITY_CLASSIFICATION ( '', '', #4521 ) ;
#2324 = CALENDAR_DATE ( 2026, 31, 10 ) ;
#2325 = CARTESIAN_POINT ( 'NONE',  ( 37.42777593783879553, 8.782604430957221098, -8.987168322345961968 ) ) ;
#2326 = CC_DESIGN_PERSON_AND_ORGANIZATION_ASSIGNMENT ( #6309, #13549, ( #12504 ) ) ;
#2327 = EDGE_CURVE ( 'NONE', #7180, #2526, #16151, .T. ) ;
#2328 = PERSON_AND_ORGANIZATION ( #3381, #3482 ) ;
#2329 = DIRECTION ( 'NONE',  ( -0.07397971354964408275, -0.9972597464969258363, 2.255140518769849223E-15 ) ) ;
#2330 = LOCAL_TIME ( 14, 11, 27.00000000000000000, #14102 ) ;
#2331 = APPLICATION_CONTEXT ( 'configuration controlled 3d designs of mechanical parts and assemblies' ) ;
#2332 = CARTESIAN_POINT ( 'NONE',  ( 35.88249351768550355, 10.99110981181060076, -10.50000000000050093 ) ) ;
#2333 = ORIENTED_EDGE ( 'NONE', *, *, #15603, .F. ) ;
#2334 = DIRECTION ( 'NONE',  ( 3.211814849206744928E-17, -2.442368445299930211E-15, -1.000000000000000000 ) ) ;
#2335 = VERTEX_POINT ( 'NONE', #1718 ) ;
#2336 = DIRECTION ( 'NONE',  ( 1.000000000000000000, 6.662111938308250026E-09, -2.269747459936919981E-13 ) ) ;
#2337 = APPROVAL_PERSON_ORGANIZATION ( #23099, #14012, #17315 ) ;
#2338 = CARTESIAN_POINT ( 'NONE',  ( -69.91240388362392366, 7.634045827809349483, 7.200000000000000178 ) ) ;
#2339 = VERTEX_POINT ( 'NONE', #9206 ) ;
#2340 = CARTESIAN_POINT ( 'NONE',  ( 60.58686099915964718, 8.989428683274725884, 3.765625566660095716E-14 ) ) ;
#2341 = DIRECTION ( 'NONE',  ( -3.099353312215988811E-62, 0.000000000000000000, 1.000000000000000000 ) ) ;
#2342 = ORIENTED_EDGE ( 'NONE', *, *, #977, .T. ) ;
#2343 = ADVANCED_FACE ( 'NONE', ( #10785 ), #5280, .F. ) ;
#2344 = APPROVAL_STATUS ( 'not_yet_approved' ) ;
#2345 = LINE ( 'NONE', #8051, #1208 ) ;
#2346 = ORGANIZATION ( 'NAUO-ORG29', 'UNSPECIFIED', 'UNSPECIFIED' ) ;
#2347 = VERTEX_POINT ( 'NONE', #5753 ) ;
#2348 = COORDINATED_UNIVERSAL_TIME_OFFSET ( 0, 0, .AHEAD. ) ;
#2349 = DIRECTION ( 'NONE',  ( -0.9730401042858024541, 0.2306359803922080898, 5.959266323854002210E-17 ) ) ;
#2350 = ORIENTED_EDGE ( 'NONE', *, *, #3124, .F. ) ;
#2351 = ORIENTED_EDGE ( 'NONE', *, *, #20302, .T. ) ;
#2352 = FACE_OUTER_BOUND ( 'NONE', #8437, .T. ) ;
#2353 = PERSON_AND_ORGANIZATION_ROLE ( 'design_supplier' ) ;
#2354 = APPROVAL_PERSON_ORGANIZATION ( #20551, #5463, #13203 ) ;
#2355 = APPROVAL_ROLE ( '' ) ;
#2356 = DIRECTION ( 'NONE',  ( -0.9730401042858024541, 0.2306359803922080898, 5.959266323858942451E-17 ) ) ;
#2357 = CIRCLE ( 'NONE', #2741, 2.009239999999998805 ) ;
#2358 = AXIS2_PLACEMENT_3D ( 'NONE', #22047, #16474, #14590 ) ;
#2359 = AXIS2_PLACEMENT_3D ( 'NONE', #21399, #12621, #2110 ) ;
#2360 = VECTOR ( 'NONE', #21663, 1000.000000000000114 ) ;
#2361 = CC_DESIGN_SECURITY_CLASSIFICATION ( #18637, ( #23509 ) ) ;
#2362 = DIRECTION ( 'NONE',  ( 0.005235963827108352890, -0.9999862922474493931, -5.936218956694023463E-19 ) ) ;
#2363 = VECTOR ( 'NONE', #13809, 1000.000000000000000 ) ;
#2364 = APPROVAL_STATUS ( 'not_yet_approved' ) ;
#2365 = VECTOR ( 'NONE', #12130, 999.9999999999998863 ) ;
#2366 = ORIENTED_EDGE ( 'NONE', *, *, #4147, .T. ) ;
#2367 = DIRECTION ( 'NONE',  ( -0.9730401042858022320, 0.2306359803922080343, 5.959266323858941219E-17 ) ) ;
#2368 = VERTEX_POINT ( 'NONE', #7430 ) ;
#2369 = ADVANCED_FACE ( 'NONE', ( #18009 ), #8578, .F. ) ;
#2370 = APPROVAL_PERSON_ORGANIZATION ( #19565, #23437, #4609 ) ;
#2371 = DIRECTION ( 'NONE',  ( 0.000000000000000000, 3.098432463554639601E-31, 1.000000000000000000 ) ) ;
#2372 = DIRECTION ( 'NONE',  ( -1.000000000000000000, -6.662112528310618598E-09, 2.269018306577664942E-13 ) ) ;
#2373 = PLANE ( 'NONE',  #9623 ) ;
#2374 = ORIENTED_EDGE ( 'NONE', *, *, #5600, .F. ) ;
#2375 = VERTEX_POINT ( 'NONE', #23445 ) ;
#2376 = FACE_BOUND ( 'NONE', #19336, .T. ) ;
#2377 = AXIS2_PLACEMENT_3D ( 'NONE', #17122, #16763, #22218 ) ;
#2378 = VERTEX_POINT ( 'NONE', #3851 ) ;
#2379 = VECTOR ( 'NONE', #3742, 1000.000000000000227 ) ;
#2380 = APPROVAL ( #15620, 'UNKNOWN' ) ;
#2381 = APPROVAL_DATE_TIME ( #6296, #16341 ) ;
#2382 = ORIENTED_EDGE ( 'NONE', *, *, #21827, .T. ) ;
#2383 = AXIS2_PLACEMENT_3D ( 'NONE', #887, #13371, #4567 ) ;
#2384 = ORIENTED_EDGE ( 'NONE', *, *, #738, .F. ) ;
#2385 = DIRECTION ( 'NONE',  ( 0.8846153846153629319, -0.4663213712685850276, 0.000000000000000000 ) ) ;
#2386 = DATE_TIME_ROLE ( 'creation_date' ) ;
#2387 = EDGE_CURVE ( 'NONE', #9101, #2031, #8977, .T. ) ;
#2388 = CARTESIAN_POINT ( 'NONE',  ( -23.49917714535037661, 22.87619892134627975, -3.750000000000000000 ) ) ;
#2389 = EDGE_CURVE ( 'NONE', #8564, #22253, #7435, .T. ) ;
#2390 = AXIS2_PLACEMENT_3D ( 'NONE', #19292, #6713, #21419 ) ;
#2391 = CARTESIAN_POINT ( 'NONE',  ( 1.358598381910800010E-16, -1.434096706618689895E-15, 8.874009851233079243E-14 ) ) ;
#2392 = VECTOR ( 'NONE', #21709, 1000.000000000000000 ) ;
#2393 = AXIS2_PLACEMENT_3D ( 'NONE', #18291, #20303, #325 ) ;
#2394 = EDGE_CURVE ( 'NONE', #14881, #6574, #5522, .T. ) ;
#2395 = SECURITY_CLASSIFICATION ( '', '', #3750 ) ;
#2396 =( LENGTH_UNIT ( ) NAMED_UNIT ( * ) SI_UNIT ( .MILLI., .METRE. ) );
#2397 = CIRCLE ( 'NONE', #19868, 4.399999999999997691 ) ;
#2398 = CIRCLE ( 'NONE', #14540, 1.749999999999997780 ) ;
#2399 = VERTEX_POINT ( 'NONE', #12774 ) ;
#2400 = DIRECTION ( 'NONE',  ( -1.000000000000000000, 0.000000000000000000, 0.000000000000000000 ) ) ;
#2401 = APPROVAL_DATE_TIME ( #13212, #6401 ) ;
#2402 = CIRCLE ( 'NONE', #11162, 2.500000000000000444 ) ;
#2403 = ORIENTED_EDGE ( 'NONE', *, *, #12336, .T. ) ;
#2404 = CARTESIAN_POINT ( 'NONE',  ( 26.57755037370660034, -6.586732293729930632, 18.00000000000000000 ) ) ;
#2405 = LINE ( 'NONE', #11576, #12048 ) ;
#2406 = ORIENTED_EDGE ( 'NONE', *, *, #6355, .T. ) ;
#2407 = EDGE_CURVE ( 'NONE', #22253, #8564, #18825, .T. ) ;
#2408 = CARTESIAN_POINT ( 'NONE',  ( 32.57408586390378247, 18.71231041770077397, -13.00000000000030020 ) ) ;
#2409 = CARTESIAN_POINT ( 'NONE',  ( 113.4570673249340018, -28.10438863268850085, 3.399999999999999911 ) ) ;
#2410 = ORIENTED_EDGE ( 'NONE', *, *, #12741, .T. ) ;
#2411 = AXIS2_PLACEMENT_3D ( 'NONE', #38, #9200, #14303 ) ;
#2412 = FACE_BOUND ( 'NONE', #4820, .T. ) ;
#2413 = APPROVAL ( #20378, 'UNSPECIFIED' ) ;
#2414 = APPROVAL_STATUS ( 'not_yet_approved' ) ;
#2415 = LOCAL_TIME ( 14, 11, 27.00000000000000000, #4197 ) ;
#2416 = AXIS2_PLACEMENT_3D ( 'NONE', #16687, #6014, #20384 ) ;
#2417 = VERTEX_POINT ( 'NONE', #14313 ) ;
#2418 = PRODUCT_RELATED_PRODUCT_CATEGORY ( 'detail', '', ( #21217 ) ) ;
#2419 = ORIENTED_EDGE ( 'NONE', *, *, #15064, .T. ) ;
#2420 = CARTESIAN_POINT ( 'NONE',  ( 31.14187293219668362, -1.979315439058181747, -15.00000000000039257 ) ) ;
#2421 = CARTESIAN_POINT ( 'NONE',  ( 38.38367524009456844, -0.1357311590789566647, -1.248138659420871028E-15 ) ) ;
#2422 = VERTEX_POINT ( 'NONE', #14427 ) ;
#2423 = AXIS2_PLACEMENT_3D ( 'NONE', #16664, #22929, #18596 ) ;
#2424 = COORDINATED_UNIVERSAL_TIME_OFFSET ( 0, 0, .AHEAD. ) ;
#2425 = EDGE_CURVE ( 'NONE', #10416, #1644, #2500, .T. ) ;
#2426 = CARTESIAN_POINT ( 'NONE',  ( 31.45181451370270054, 16.90945435098589655, 23.00000000000000000 ) ) ;
#2427 = EDGE_CURVE ( 'NONE', #1783, #13768, #6680, .T. ) ;
#2428 = CC_DESIGN_DATE_AND_TIME_ASSIGNMENT ( #1531, #12262, ( #9941 ) ) ;
#2429 = CARTESIAN_POINT ( 'NONE',  ( -13.66074082773489984, 1.277408929928570025, 2.500000000000000000 ) ) ;
#2430 = CONTEXT_DEPENDENT_SHAPE_REPRESENTATION ( #7637, #22576 ) ;
#2431 = DIRECTION ( 'NONE',  ( -0.9730401042858024541, 0.2306359803922080898, 5.959266323858942451E-17 ) ) ;
#2432 =( LENGTH_UNIT ( ) NAMED_UNIT ( * ) SI_UNIT ( .MILLI., .METRE. ) );
#2433 = DIRECTION ( 'NONE',  ( 3.099353312215989243E-62, -1.534091707905539548E-92, -1.000000000000000000 ) ) ;
#2434 = CARTESIAN_POINT ( 'NONE',  ( -17.50000000397270128, 22.95208920922877738, 5.500000000004431122 ) ) ;
#2435 = DATE_AND_TIME ( #13122, #13317 ) ;
#2436 = VECTOR ( 'NONE', #22132, 1000.000000000000000 ) ;
#2437 = CARTESIAN_POINT ( 'NONE',  ( -14.00000000202700079, 1.899127378930349996, -6.749999999996879829 ) ) ;
#2438 = AXIS2_PLACEMENT_3D ( 'NONE', #18783, #1291, #17921 ) ;
#2439 = LINE ( 'NONE', #9694, #22667 ) ;
#2440 = CARTESIAN_POINT ( 'NONE',  ( 37.10730959030829723, 23.96304573415810069, -11.00000000000049916 ) ) ;
#2441 = EDGE_CURVE ( 'NONE', #13655, #6050, #20011, .T. ) ;
#2442 = FACE_OUTER_BOUND ( 'NONE', #2247, .T. ) ;
#2443 = CARTESIAN_POINT ( 'NONE',  ( -20.00000000000000000, -20.00000000000000000, -4.999999999995470290 ) ) ;
#2444 = FACE_OUTER_BOUND ( 'NONE', #4660, .T. ) ;
#2445 = VERTEX_POINT ( 'NONE', #16440 ) ;
#2446 = EDGE_LOOP ( 'NONE', ( #5785, #15604, #21609, #12000 ) ) ;
#2447 = PLANE ( 'NONE',  #13761 ) ;
#2448 = DIRECTION ( 'NONE',  ( 1.000000000000000000, 0.000000000000000000, 0.000000000000000000 ) ) ;
#2449 = ORIENTED_EDGE ( 'NONE', *, *, #21301, .T. ) ;
#2450 = EDGE_CURVE ( 'NONE', #13217, #14219, #21981, .T. ) ;
#2451 = DIRECTION ( 'NONE',  ( 0.7806762821593219437, -0.6249356306643899517, -1.759009604640482394E-13 ) ) ;
#2452 = ORIENTED_EDGE ( 'NONE', *, *, #10875, .T. ) ;
#2453 = ADVANCED_FACE ( 'NONE', ( #18362 ), #2071, .F. ) ;
#2454 = FACE_OUTER_BOUND ( 'NONE', #19325, .T. ) ;
#2455 =( BOUNDED_CURVE ( )  B_SPLINE_CURVE ( 2, ( #20488, #291, #2201 ),
 .UNSPECIFIED., .F., .F. ) 
 B_SPLINE_CURVE_WITH_KNOTS ( ( 3, 3 ),
 ( 0.000000000000000000, 0.2336872276155859962 ),
 .UNSPECIFIED. ) 
 CURVE ( )  GEOMETRIC_REPRESENTATION_ITEM ( )  RATIONAL_B_SPLINE_CURVE ( ( 1.000000000000000000, 1.154700538379259900, 1.000000000000000000 ) ) 
 REPRESENTATION_ITEM ( '' )  );
#2456 = DATE_TIME_ROLE ( 'creation_date' ) ;
#2457 = CARTESIAN_POINT ( 'NONE',  ( 38.22140682376687693, 9.152092534394331125, -26.50000000000049383 ) ) ;
#2458 = APPROVAL_ROLE ( '' ) ;
#2459 = DIRECTION ( 'NONE',  ( -0.9999862922474492821, -0.005235963827121951387, 1.187304881134294758E-16 ) ) ;
#2460 = EDGE_LOOP ( 'NONE', ( #23245, #9705 ) ) ;
#2461 = DIRECTION ( 'NONE',  ( 5.798605125234323991E-17, -1.374421231021384554E-17, 1.000000000000000000 ) ) ;
#2462 = ORIENTED_EDGE ( 'NONE', *, *, #10309, .F. ) ;
#2463 = FACE_OUTER_BOUND ( 'NONE', #13108, .T. ) ;
#2464 = LINE ( 'NONE', #8162, #21625 ) ;
#2465 = ORIENTED_EDGE ( 'NONE', *, *, #11732, .F. ) ;
#2466 = CARTESIAN_POINT ( 'NONE',  ( 35.11747397072455357, 7.763535785894623231, -8.759424124906624698 ) ) ;
#2467 = FACE_OUTER_BOUND ( 'NONE', #7732, .T. ) ;
#2468 = EDGE_LOOP ( 'NONE', ( #8073, #14635, #15259, #20781 ) ) ;
#2469 = CIRCLE ( 'NONE', #13848, 2.499999999999998224 ) ;
#2470 = PERSON_AND_ORGANIZATION_ROLE ( 'classification_officer' ) ;
#2471 = CARTESIAN_POINT ( 'NONE',  ( -25.00000000000000000, -20.00000000000000000, -2.500000000000000000 ) ) ;
#2472 = ADVANCED_FACE ( 'NONE', ( #21544 ), #16320, .F. ) ;
#2473 = ORIENTED_EDGE ( 'NONE', *, *, #13290, .T. ) ;
#2474 = ADVANCED_FACE ( 'NONE', ( #44 ), #21786, .T. ) ;
#2475 = APPROVAL_DATE_TIME ( #6146, #10855 ) ;
#2476 = CARTESIAN_POINT ( 'NONE',  ( -16.50058068176714343, 23.02794805996801841, 2.499999999999950262 ) ) ;
#2477 = EDGE_LOOP ( 'NONE', ( #22469, #21912, #14878, #15493 ) ) ;
#2478 = ORIENTED_EDGE ( 'NONE', *, *, #17643, .F. ) ;
#2479 = CARTESIAN_POINT ( 'NONE',  ( 50.90756547144189881, 18.01515514085709668, 3.544128957608909560E-14 ) ) ;
#2480 = PERSON_AND_ORGANIZATION ( #11966, #8758 ) ;
#2481 = VECTOR ( 'NONE', #17324, 1000.000000000000114 ) ;
#2482 = DATE_TIME_ROLE ( 'classification_date' ) ;
#2483 = LINE ( 'NONE', #20523, #3980 ) ;
#2484 = FACE_OUTER_BOUND ( 'NONE', #19142, .T. ) ;
#2485 = VERTEX_POINT ( 'NONE', #19901 ) ;
#2486 = DATE_AND_TIME ( #688, #7591 ) ;
#2487 = PRODUCT_DEFINITION_SHAPE ( 'NONE', 'NONE',  #23508 ) ;
#2488 = ORIENTED_EDGE ( 'NONE', *, *, #23166, .F. ) ;
#2489 = CARTESIAN_POINT ( 'NONE',  ( -20.00000000397270128, 22.95208919257349933, 6.750000000004470202 ) ) ;
#2490 = ORIENTED_EDGE ( 'NONE', *, *, #10150, .F. ) ;
#2491 = CARTESIAN_POINT ( 'NONE',  ( -57.16525610687759951, 12.70085888708699962, 5.715859474400029324E-15 ) ) ;
#2492 = AXIS2_PLACEMENT_3D ( 'NONE', #2207, #11625, #7915 ) ;
#2493 = DIRECTION ( 'NONE',  ( -0.9999862922474492821, -0.005235963827121953122, 1.239088197126291310E-16 ) ) ;
#2494 = DIRECTION ( 'NONE',  ( -0.2306359803922033158, -0.9730401042858034533, 0.000000000000000000 ) ) ;
#2495 = ORIENTED_EDGE ( 'NONE', *, *, #7190, .F. ) ;
#2496 = ORIENTED_EDGE ( 'NONE', *, *, #4549, .T. ) ;
#2497 = CARTESIAN_POINT ( 'NONE',  ( -21.66385406723090057, 11.15564796089419985, 2.500000000000000000 ) ) ;
#2498 = VERTEX_POINT ( 'NONE', #2549 ) ;
#2499 = DATE_AND_TIME ( #20664, #3820 ) ;
#2500 = CIRCLE ( 'NONE', #16901, 2.500000000000000444 ) ;
#2501 = ORIENTED_EDGE ( 'NONE', *, *, #9557, .F. ) ;
#2502 = ORIENTED_EDGE ( 'NONE', *, *, #10974, .T. ) ;
#2503 = DIRECTION ( 'NONE',  ( -0.7033367706102514605, -0.7108567978907863738, -4.197882762799809725E-19 ) ) ;
#2504 = PERSON_AND_ORGANIZATION ( #11966, #8758 ) ;
#2505 = CARTESIAN_POINT ( 'NONE',  ( 30.72899802076640086, 10.92798958341530025, -1.881607274541729715E-15 ) ) ;
#2506 = CARTESIAN_POINT ( 'NONE',  ( -56.96862724498259922, -24.85214435119530307, -5.538187069399500051E-15 ) ) ;
#2507 = ADVANCED_FACE ( 'NONE', ( #13478, #7779, #20711 ), #11607, .F. ) ;
#2508 = EDGE_CURVE ( 'NONE', #10083, #7364, #5527, .T. ) ;
#2509 = SHAPE_REPRESENTATION ( '1602p_c_45', ( #12739 ), #1146 ) ;
#2510 = AXIS2_PLACEMENT_3D ( 'NONE', #8914, #7022, #19484 ) ;
#2511 = DIRECTION ( 'NONE',  ( 0.000000000000000000, 0.000000000000000000, 1.000000000000000000 ) ) ;
#2512 = APPROVAL_STATUS ( 'not_yet_approved' ) ;
#2513 = ORIENTED_EDGE ( 'NONE', *, *, #17946, .F. ) ;
#2514 = CARTESIAN_POINT ( 'NONE',  ( -65.82539143210260590, 12.65551411021120032, 5.000000000000000000 ) ) ;
#2515 = CARTESIAN_POINT ( 'NONE',  ( -14.00000000202730099, 1.899127378930349996, -7.999999999996879829 ) ) ;
#2516 = ORIENTED_EDGE ( 'NONE', *, *, #4438, .T. ) ;
#2517 = ADVANCED_FACE ( 'NONE', ( #7893 ), #20255, .F. ) ;
#2518 = EDGE_CURVE ( 'NONE', #12383, #14944, #18829, .T. ) ;
#2519 = CYLINDRICAL_SURFACE ( 'NONE', #15830, 5.000000000000001776 ) ;
#2520 = CYLINDRICAL_SURFACE ( 'NONE', #6156, 2.499999999999999112 ) ;
#2521 = ORIENTED_EDGE ( 'NONE', *, *, #13591, .T. ) ;
#2522 = CARTESIAN_POINT ( 'NONE',  ( 34.94102482032229773, 25.66320561742219653, 13.00000000000000000 ) ) ;
#2523 = SECURITY_CLASSIFICATION_LEVEL ( 'unclassified' ) ;
#2524 = AXIS2_PLACEMENT_3D ( 'NONE', #13314, #15206, #16868 ) ;
#2525 = ORIENTED_EDGE ( 'NONE', *, *, #8870, .F. ) ;
#2526 = VERTEX_POINT ( 'NONE', #16661 ) ;
#2527 = CARTESIAN_POINT ( 'NONE',  ( 34.40556712239440174, 8.514986143070938596, -29.25000000000050093 ) ) ;
#2528 = AXIS2_PLACEMENT_3D ( 'NONE', #22951, #3244, #15948 ) ;
#2529 = CARTESIAN_POINT ( 'NONE',  ( 31.56827854690370927, -0.8510906712623020898, -12.00000000000039968 ) ) ;
#2530 = ORIENTED_EDGE ( 'NONE', *, *, #8422, .T. ) ;
#2531 = APPROVAL_STATUS ( 'not_yet_approved' ) ;
#2532 = DIRECTION ( 'NONE',  ( 6.124378941434239724E-17, -2.274246353359159970E-33, 1.000000000000000000 ) ) ;
#2533 = FACE_OUTER_BOUND ( 'NONE', #11728, .T. ) ;
#2534 = APPROVAL_DATE_TIME ( #9794, #12001 ) ;
#2535 = DIRECTION ( 'NONE',  ( -1.466984912809907930E-16, -2.805478249466190329E-20, -1.000000000000000000 ) ) ;
#2536 = EDGE_CURVE ( 'NONE', #14624, #1110, #11252, .T. ) ;
#2537 = FACE_OUTER_BOUND ( 'NONE', #13025, .T. ) ;
#2538 = APPROVAL ( #12762, 'UNSPECIFIED' ) ;
#2539 = DIRECTION ( 'NONE',  ( -0.2306359803922033713, -0.9730401042858033422, 1.407521210652564805E-17 ) ) ;
#2540 = APPROVAL_DATE_TIME ( #2435, #5101 ) ;
#2541 = AXIS2_PLACEMENT_3D ( 'NONE', #2566, #4466, #997 ) ;
#2542 = APPROVAL ( #2885, 'UNSPECIFIED' ) ;
#2543 = VECTOR ( 'NONE', #10216, 1000.000000000000114 ) ;
#2544 = AXIS2_PLACEMENT_3D ( 'NONE', #13583, #20824, #4554 ) ;
#2545 = CARTESIAN_POINT ( 'NONE',  ( -17.50058776013304396, 23.00629652915649004, -2.500000000000039968 ) ) ;
#2546 = CARTESIAN_POINT ( 'NONE',  ( -0.5391976746782148888, 18.33937061236850141, 3.301631463538509622E-17 ) ) ;
#2547 = ADVANCED_FACE ( 'NONE', ( #15124, #13010, #4445 ), #874, .F. ) ;
#2548 = EDGE_CURVE ( 'NONE', #15489, #19229, #2146, .T. ) ;
#2549 = CARTESIAN_POINT ( 'NONE',  ( -17.50000000000000000, -20.00000000000000000, -5.000000000000000000 ) ) ;
#2550 = CARTESIAN_POINT ( 'NONE',  ( 37.46113131852554545, -4.027891576223090020, -13.00000000000000000 ) ) ;
#2551 = DIRECTION ( 'NONE',  ( -6.123237831918399306E-17, 1.569224110909209817E-30, 1.000000000000000000 ) ) ;
#2552 = EDGE_LOOP ( 'NONE', ( #3963, #3451, #20173, #11611 ) ) ;
#2553 = ADVANCED_BREP_SHAPE_REPRESENTATION ( '', ( #17389, #12739 ), #10500 ) ;
#2554 = ORIENTED_EDGE ( 'NONE', *, *, #6613, .T. ) ;
#2555 = DIRECTION ( 'NONE',  ( -6.662161563160872600E-09, 1.000000000000000000, -1.982541115402066096E-15 ) ) ;
#2556 = CARTESIAN_POINT ( 'NONE',  ( 31.01827548281339020, -2.500766059351137827, -15.00000000000039613 ) ) ;
#2557 = AXIS2_PLACEMENT_3D ( 'NONE', #7288, #23418, #3821 ) ;
#2558 = ORIENTED_EDGE ( 'NONE', *, *, #1179, .F. ) ;
#2559 = DIRECTION ( 'NONE',  ( 0.000000000000000000, 1.000000000000000000, 0.000000000000000000 ) ) ;
#2560 = AXIS2_PLACEMENT_3D ( 'NONE', #12570, #9240, #16122 ) ;
#2561 = VERTEX_POINT ( 'NONE', #2440 ) ;
#2562 = CIRCLE ( 'NONE', #5585, 0.4000000000000010214 ) ;
#2563 = LINE ( 'NONE', #10294, #3032 ) ;
#2564 = AXIS2_PLACEMENT_3D ( 'NONE', #14489, #1535, #12376 ) ;
#2565 = PERSON_AND_ORGANIZATION_ROLE ( 'creator' ) ;
#2566 = CARTESIAN_POINT ( 'NONE',  ( 43.87899317387989839, 21.17128575569940097, -13.00000000000000000 ) ) ;
#2567 = EDGE_CURVE ( 'NONE', #9360, #6052, #5928, .T. ) ;
#2568 = COORDINATED_UNIVERSAL_TIME_OFFSET ( 0, 0, .AHEAD. ) ;
#2569 = CARTESIAN_POINT ( 'NONE',  ( 0.000000000000000000, 0.000000000000000000, 0.000000000000000000 ) ) ;
#2570 = CARTESIAN_POINT ( 'NONE',  ( -62.82872441665805496, -8.329083101359751495, -5.528360538656856695E-15 ) ) ;
#2571 = CC_DESIGN_PERSON_AND_ORGANIZATION_ASSIGNMENT ( #7273, #16399, ( #2832 ) ) ;
#2572 = AXIS2_PLACEMENT_3D ( 'NONE', #959, #8217, #13673 ) ;
#2573 = LINE ( 'NONE', #9830, #4320 ) ;
#2574 = ORIENTED_EDGE ( 'NONE', *, *, #11403, .F. ) ;
#2575 = DIRECTION ( 'NONE',  ( 0.005235963827108302583, -0.9999862922474493931, -5.936218956694023463E-19 ) ) ;
#2576 = EDGE_CURVE ( 'NONE', #22163, #22602, #10894, .T. ) ;
#2577 = EDGE_CURVE ( 'NONE', #20612, #14607, #14899, .T. ) ;
#2578 = AXIS2_PLACEMENT_3D ( 'NONE', #1717, #12540, #18230 ) ;
#2579 = CARTESIAN_POINT ( 'NONE',  ( -67.06978017061331343, -25.35162245663349978, -2.500000000000000000 ) ) ;
#2580 = AXIS2_PLACEMENT_3D ( 'NONE', #17763, #21435, #14658 ) ;
#2581 = ORIENTED_EDGE ( 'NONE', *, *, #9104, .F. ) ;
#2582 = LINE ( 'NONE', #13267, #22238 ) ;
#2583 = PLANE ( 'NONE',  #9142 ) ;
#2584 = ORIENTED_EDGE ( 'NONE', *, *, #5694, .T. ) ;
#2585 = DATE_AND_TIME ( #16946, #9586 ) ;
#2586 = DIRECTION ( 'NONE',  ( 1.524428182562999945E-15, 6.173091865707990781E-15, 1.000000000000000000 ) ) ;
#2587 =( BOUNDED_CURVE ( )  B_SPLINE_CURVE ( 2, ( #19385, #13684, #8344 ),
 .UNSPECIFIED., .F., .T. ) 
 B_SPLINE_CURVE_WITH_KNOTS ( ( 3, 3 ),
 ( 0.000000000000000000, 0.5842180690389588982 ),
 .UNSPECIFIED. ) 
 CURVE ( )  GEOMETRIC_REPRESENTATION_ITEM ( )  RATIONAL_B_SPLINE_CURVE ( ( 1.000000000000000000, 1.154700538379249908, 1.000000000000000000 ) ) 
 REPRESENTATION_ITEM ( '' )  );
#2588 = VERTEX_POINT ( 'NONE', #13125 ) ;
#2589 = PERSON_AND_ORGANIZATION_ROLE ( 'creator' ) ;
#2590 = DIRECTION ( 'NONE',  ( 6.123237831918399306E-17, -1.590047762086094914E-30, -1.000000000000000000 ) ) ;
#2591 = VERTEX_POINT ( 'NONE', #18592 ) ;
#2592 = VERTEX_POINT ( 'NONE', #2308 ) ;
#2593 = VECTOR ( 'NONE', #5932, 1000.000000000000000 ) ;
#2594 = COORDINATED_UNIVERSAL_TIME_OFFSET ( 0, 0, .AHEAD. ) ;
#2595 = EDGE_CURVE ( 'NONE', #15865, #13888, #5991, .T. ) ;
#2596 = APPROVAL_STATUS ( 'not_yet_approved' ) ;
#2597 = VECTOR ( 'NONE', #1447, 999.9999999999998863 ) ;
#2598 = LINE ( 'NONE', #8062, #941 ) ;
#2599 = EDGE_CURVE ( 'NONE', #1608, #8149, #11245, .T. ) ;
#2600 = CARTESIAN_POINT ( 'NONE',  ( -32.64682763696299617, 7.329162855357659545, -2.500000000000000000 ) ) ;
#2601 = EDGE_LOOP ( 'NONE', ( #3077, #13801 ) ) ;
#2602 = APPLICATION_CONTEXT ( 'configuration controlled 3d designs of mechanical parts and assemblies' ) ;
#2603 = EDGE_CURVE ( 'NONE', #22277, #21097, #4428, .T. ) ;
#2604 = PERSON_AND_ORGANIZATION_ROLE ( 'creator' ) ;
#2605 = EDGE_CURVE ( 'NONE', #22018, #17928, #909, .T. ) ;
#2606 = ORIENTED_EDGE ( 'NONE', *, *, #14710, .T. ) ;
#2607 = DIRECTION ( 'NONE',  ( 0.000000000000000000, 1.000000000000000000, 0.000000000000000000 ) ) ;
#2608 = CARTESIAN_POINT ( 'NONE',  ( -26.68881687192900287, -6.639832696913689603, -2.500292893218899692 ) ) ;
#2609 = VERTEX_POINT ( 'NONE', #16912 ) ;
#2610 = CARTESIAN_POINT ( 'NONE',  ( -30.75845054331819739, -0.1610523420890289936, 2.999000000000090260 ) ) ;
#2612 = VECTOR ( 'NONE', #831, 1000.000000000000000 ) ;
#2611 = CARTESIAN_POINT ( 'NONE',  ( -27.50000000434449987, 26.95208919188010199, -7.999999999993869793 ) ) ;
#2613 = DIRECTION ( 'NONE',  ( -6.123230174520380038E-17, -4.962644601432250805E-15, -1.000000000000000000 ) ) ;
#2614 = ORIENTED_EDGE ( 'NONE', *, *, #15857, .F. ) ;
#2615 = ORIENTED_EDGE ( 'NONE', *, *, #11565, .T. ) ;
#2616 = CYLINDRICAL_SURFACE ( 'NONE', #4170, 5.000000000000001776 ) ;
#2617 = ORIENTED_EDGE ( 'NONE', *, *, #17945, .T. ) ;
#2618 = APPLICATION_PROTOCOL_DEFINITION ( 'international standard', 'config_control_design', 1994, #21752 ) ;
#2619 = ORIENTED_EDGE ( 'NONE', *, *, #11412, .F. ) ;
#2620 = VERTEX_POINT ( 'NONE', #6707 ) ;
#2621 = LINE ( 'NONE', #13200, #9974 ) ;
#2622 = PERSON_AND_ORGANIZATION ( #11966, #8758 ) ;
#2623 = DIRECTION ( 'NONE',  ( 0.2306359803922028995, 0.9730401042858036753, -9.756037151021835575E-16 ) ) ;
#2624 = CARTESIAN_POINT ( 'NONE',  ( 30.31182762792540331, -4.706706774123539994, -13.00000000000039968 ) ) ;
#2625 = APPROVAL ( #18083, 'UNSPECIFIED' ) ;
#2626 = SHAPE_REPRESENTATION_RELATIONSHIP ( 'NONE' , 'NONE' ,  #21569, #3149 ) ;
#2627 = CARTESIAN_POINT ( 'NONE',  ( 35.59419854219520118, 9.774809681453278998, -23.00000000000000000 ) ) ;
#2628 = APPROVAL_ROLE ( '' ) ;
#2629 = VERTEX_POINT ( 'NONE', #21063 ) ;
#2630 = LOCAL_TIME ( 14, 11, 27.00000000000000000, #17075 ) ;
#2631 = CARTESIAN_POINT ( 'NONE',  ( -14.70588235717659842, 25.77561860482770228, -6.749999999996769695 ) ) ;
#2632 = VECTOR ( 'NONE', #22694, 1000.000000000000000 ) ;
#2633 = LINE ( 'NONE', #9889, #648 ) ;
#2634 = ORIENTED_EDGE ( 'NONE', *, *, #18406, .F. ) ;
#2635 = CARTESIAN_POINT ( 'NONE',  ( 80.84056339148629888, -0.9497634067828859550, 3.641582893490300021E-14 ) ) ;
#2636 = CARTESIAN_POINT ( 'NONE',  ( -2.966462739374829791E-16, -7.772954297906289827E-16, -2.500000000000090150 ) ) ;
#2637 = ORIENTED_EDGE ( 'NONE', *, *, #5444, .T. ) ;
#2638 = DIRECTION ( 'NONE',  ( 0.000000000000000000, 0.000000000000000000, 1.000000000000000000 ) ) ;
#2639 = DATE_TIME_ROLE ( 'creation_date' ) ;
#2640 = ADVANCED_FACE ( 'NONE', ( #5036 ), #15723, .T. ) ;
#2641 = VERTEX_POINT ( 'NONE', #10053 ) ;
#2642 = ORIENTED_EDGE ( 'NONE', *, *, #3233, .F. ) ;
#2643 = CYLINDRICAL_SURFACE ( 'NONE', #6583, 5.000000000000000000 ) ;
#2644 = CYLINDRICAL_SURFACE ( 'NONE', #11382, 5.000000000000000888 ) ;
#2645 = DIRECTION ( 'NONE',  ( -0.7070970883417637687, -0.003702385528197199398, -0.7071067811865480168 ) ) ;
#2646 = PERSON_AND_ORGANIZATION_ROLE ( 'creator' ) ;
#2647 = LINE ( 'NONE', #2426, #1624 ) ;
#2648 = CARTESIAN_POINT ( 'NONE',  ( -3.458317987535629801, 19.03127855354509990, -7.892745253163399067E-16 ) ) ;
#2649 = AXIS2_PLACEMENT_3D ( 'NONE', #10619, #17847, #1561 ) ;
#2650 = DATE_AND_TIME ( #20704, #3017 ) ;
#2651 = CIRCLE ( 'NONE', #14410, 5.000000000000004441 ) ;
#2652 = CARTESIAN_POINT ( 'NONE',  ( -20.00000000000000000, -20.00000000000000000, -2.500000000000000000 ) ) ;
#2653 = AXIS2_PLACEMENT_3D ( 'NONE', #22839, #8363, #3007 ) ;
#2654 = CARTESIAN_POINT ( 'NONE',  ( 41.15130700480209924, 11.54075009235119964, 15.90000000000000036 ) ) ;
#2655 = DATE_AND_TIME ( #13934, #18629 ) ;
#2656 = CARTESIAN_POINT ( 'NONE',  ( -20.00000000397270128, 22.95208919256889857, -2.500000000000000000 ) ) ;
#2657 = CARTESIAN_POINT ( 'NONE',  ( 34.88044566782579636, 28.44271146055880095, -18.00000000000029843 ) ) ;
#2658 = CARTESIAN_POINT ( 'NONE',  ( -67.24235627552212691, 7.607684554713951997, -2.500000000000000000 ) ) ;
#2659 = APPROVAL_PERSON_ORGANIZATION ( #11925, #4793, #2865 ) ;
#2660 = CARTESIAN_POINT ( 'NONE',  ( -27.00000000000000000, -31.09999999999999787, -21.50000000000000000 ) ) ;
#2661 = FACE_OUTER_BOUND ( 'NONE', #11316, .T. ) ;
#2662 = APPROVAL_PERSON_ORGANIZATION ( #16752, #8156, #20085 ) ;
#2663 = CARTESIAN_POINT ( 'NONE',  ( -0.001390367605393909908, 20.60834910077250015, 4.500000000000000000 ) ) ;
#2664 = ORIENTED_EDGE ( 'NONE', *, *, #5584, .F. ) ;
#2665 = ADVANCED_FACE ( 'NONE', ( #20827 ), #6455, .T. ) ;
#2666 = VERTEX_POINT ( 'NONE', #17277 ) ;
#2667 = CARTESIAN_POINT ( 'NONE',  ( 26.57755037370649731, -6.586732293730120702, -18.00000000000000000 ) ) ;
#2668 = DIRECTION ( 'NONE',  ( 7.252994924361790472E-16, -5.047364287626240282E-15, -1.000000000000000000 ) ) ;
#2669 = EDGE_LOOP ( 'NONE', ( #11938, #9938 ) ) ;
#2670 = VECTOR ( 'NONE', #16410, 1000.000000000000000 ) ;
#2671 = CC_DESIGN_PERSON_AND_ORGANIZATION_ASSIGNMENT ( #1991, #3891, ( #8052 ) ) ;
#2672 = DIRECTION ( 'NONE',  ( 2.269747459788994803E-13, 2.220446049250715400E-15, 1.000000000000000000 ) ) ;
#2673 = ORIENTED_EDGE ( 'NONE', *, *, #8047, .F. ) ;
#2674 = CYLINDRICAL_SURFACE ( 'NONE', #7218, 3.499999999999998668 ) ;
#2675 = CIRCLE ( 'NONE', #16693, 4.250000000000001776 ) ;
#2676 = APPLICATION_PROTOCOL_DEFINITION ( 'international standard', 'config_control_design', 1994, #16698 ) ;
#2677 = CARTESIAN_POINT ( 'NONE',  ( -67.33861934291638818, 12.64759079499718375, 3.945395128240059864E-15 ) ) ;
#2678 = EDGE_CURVE ( 'NONE', #6764, #11726, #1747, .T. ) ;
#2679 = ADVANCED_FACE ( 'NONE', ( #1096 ), #13586, .T. ) ;
#2680 = PRODUCT_DEFINITION_SHAPE ( 'NONE', 'NONE',  #23475 ) ;
#2681 = LOCAL_TIME ( 14, 11, 27.00000000000000000, #11344 ) ;
#2682 = CALENDAR_DATE ( 2026, 31, 10 ) ;
#2683 =( NAMED_UNIT ( * ) PLANE_ANGLE_UNIT ( ) SI_UNIT ( $, .RADIAN. ) );
#2684 = APPROVAL_PERSON_ORGANIZATION ( #12110, #17381, #4960 ) ;
#2685 = LINE ( 'NONE', #897, #11719 ) ;
#2686 = CARTESIAN_POINT ( 'NONE',  ( 30.57814311865390167, -3.583136841839989817, 15.00000000000000000 ) ) ;
#2687 = ORIENTED_EDGE ( 'NONE', *, *, #19215, .F. ) ;
#2688 = DIRECTION ( 'NONE',  ( -3.099353312215989243E-62, -9.818186930595456717E-93, 1.000000000000000000 ) ) ;
#2689 = DIRECTION ( 'NONE',  ( 4.115594265198981899E-36, 2.805478249476870212E-20, 1.000000000000000000 ) ) ;
#2690 = ORIENTED_EDGE ( 'NONE', *, *, #20301, .T. ) ;
#2691 = DIRECTION ( 'NONE',  ( 2.977235988022388482E-185, -9.605990953944227443E-124, -1.000000000000000000 ) ) ;
#2692 = DIRECTION ( 'NONE',  ( -3.210834492181045054E-17, 2.441916418604790135E-15, 1.000000000000000000 ) ) ;
#2693 = UNCERTAINTY_MEASURE_WITH_UNIT (LENGTH_MEASURE( 1.000000000000000082E-05 ), #14712, 'distance_accuracy_value', 'NONE');
#2694 = EDGE_CURVE ( 'NONE', #6087, #1299, #14053, .T. ) ;
#2695 = CC_DESIGN_APPROVAL ( #17068, ( #13884 ) ) ;
#2696 = LINE ( 'NONE', #6496, #16825 ) ;
#2697 = CC_DESIGN_APPROVAL ( #6401, ( #11077 ) ) ;
#2698 = ORIENTED_EDGE ( 'NONE', *, *, #18662, .T. ) ;
#2700 = PERSON_AND_ORGANIZATION_ROLE ( 'creator' ) ;
#2699 = CC_DESIGN_PERSON_AND_ORGANIZATION_ASSIGNMENT ( #11622, #8031, ( #9078 ) ) ;
#2701 = DIRECTION ( 'NONE',  ( -0.2306359803922027885, -0.9730401042858034533, 4.741332172908048425E-18 ) ) ;
#2702 = VECTOR ( 'NONE', #11036, 1000.000000000000000 ) ;
#2703 = ORIENTED_EDGE ( 'NONE', *, *, #20444, .T. ) ;
#2704 = ORIENTED_EDGE ( 'NONE', *, *, #19706, .F. ) ;
#2705 = CC_DESIGN_PERSON_AND_ORGANIZATION_ASSIGNMENT ( #3636, #16777, ( #6637 ) ) ;
#2706 = DIRECTION ( 'NONE',  ( -0.2306359803921919083, -0.9730401042858062288, 0.000000000000000000 ) ) ;
#2707 = CC_DESIGN_APPROVAL ( #4717, ( #12227 ) ) ;
#2708 = APPROVAL_ROLE ( '' ) ;
#2709 = VECTOR ( 'NONE', #13240, 1000.000000000000000 ) ;
#2710 = EDGE_CURVE ( 'NONE', #17907, #2629, #10123, .T. ) ;
#2711 = ADVANCED_FACE ( 'NONE', ( #17745 ), #19402, .F. ) ;
#2712 = CC_DESIGN_PERSON_AND_ORGANIZATION_ASSIGNMENT ( #19711, #9143, ( #5117 ) ) ;
#2713 = DATE_AND_TIME ( #20872, #8411 ) ;
#2714 = CARTESIAN_POINT ( 'NONE',  ( -22.52506282043049879, 26.45208917575140006, 8.000000000004488854 ) ) ;
#2715 = CC_DESIGN_APPROVAL ( #20272, ( #5355 ) ) ;
#2716 = LOCAL_TIME ( 14, 11, 27.00000000000000000, #14487 ) ;
#2717 = DIRECTION ( 'NONE',  ( 0.9730401042858035643, -0.2306359803922028717, -5.432877459303547053E-17 ) ) ;
#2718 = AXIS2_PLACEMENT_3D ( 'NONE', #7836, #15072, #13183 ) ;
#2719 = VERTEX_POINT ( 'NONE', #983 ) ;
#2720 = AXIS2_PLACEMENT_3D ( 'NONE', #6693, #7049, #1676 ) ;
#2721 = COORDINATED_UNIVERSAL_TIME_OFFSET ( 0, 0, .AHEAD. ) ;
#2722 = ORIENTED_EDGE ( 'NONE', *, *, #23317, .F. ) ;
#2723 = CC_DESIGN_SECURITY_CLASSIFICATION ( #16748, ( #23497 ) ) ;
#2724 = CARTESIAN_POINT ( 'NONE',  ( -22.99995202268987171, -0.1204285676208978334, 2.500000000000090594 ) ) ;
#2725 = CARTESIAN_POINT ( 'NONE',  ( 118.4388045014059969, -7.086722380115130449, 18.89999999999999858 ) ) ;
#2726 = ORIENTED_EDGE ( 'NONE', *, *, #8209, .F. ) ;
#2727 = EDGE_CURVE ( 'NONE', #9837, #21452, #9750, .T. ) ;
#2728 = PLANE ( 'NONE',  #19279 ) ;
#2729 = CARTESIAN_POINT ( 'NONE',  ( -22.99995202268966921, -0.1204285676209190525, -2.499999999999999556 ) ) ;
#2730 = CARTESIAN_POINT ( 'NONE',  ( -20.00000000000149925, -20.00000000000000000, -6.499999999995289990 ) ) ;
#2731 = ORIENTED_EDGE ( 'NONE', *, *, #17971, .F. ) ;
#2732 = ORIENTED_EDGE ( 'NONE', *, *, #18565, .T. ) ;
#2733 = DIRECTION ( 'NONE',  ( 0.000000000000000000, 0.000000000000000000, 1.000000000000000000 ) ) ;
#2734 = ORIENTED_EDGE ( 'NONE', *, *, #4247, .F. ) ;
#2735 = PERSON_AND_ORGANIZATION ( #11966, #8758 ) ;
#2736 = CC_DESIGN_APPROVAL ( #9994, ( #13165 ) ) ;
#2737 = EDGE_LOOP ( 'NONE', ( #13650, #12915, #20633, #15109 ) ) ;
#2738 = ORIENTED_EDGE ( 'NONE', *, *, #11377, .F. ) ;
#2739 = CARTESIAN_POINT ( 'NONE',  ( -30.15704507771850018, 9.287077397714901039, -3.750000000000000000 ) ) ;
#2740 = MECHANICAL_CONTEXT ( 'NONE', #13089, 'mechanical' ) ;
#2741 = AXIS2_PLACEMENT_3D ( 'NONE', #1805, #17988, #8845 ) ;
#2742 = EDGE_CURVE ( 'NONE', #20392, #23222, #11283, .T. ) ;
#2743 = EDGE_CURVE ( 'NONE', #7183, #21038, #21858, .T. ) ;
#2744 = VECTOR ( 'NONE', #9735, 1000.000000000000000 ) ;
#2745 = CARTESIAN_POINT ( 'NONE',  ( 36.78282996199610722, 11.03463321983590006, 27.68999999999999773 ) ) ;
#2746 = AXIS2_PLACEMENT_3D ( 'NONE', #15981, #23093, #21331 ) ;
#2747 = APPROVAL_PERSON_ORGANIZATION ( #10424, #1209, #3155 ) ;
#2748 = AXIS2_PLACEMENT_3D ( 'NONE', #4163, #822, #7848 ) ;
#2749 = CYLINDRICAL_SURFACE ( 'NONE', #23026, 4.099999999999999645 ) ;
#2750 = DATE_TIME_ROLE ( 'classification_date' ) ;
#2751 = CC_DESIGN_SECURITY_CLASSIFICATION ( #9978, ( #1599 ) ) ;
#2752 = ORIENTED_EDGE ( 'NONE', *, *, #1218, .T. ) ;
#2753 = CARTESIAN_POINT ( 'NONE',  ( 118.5310588935630136, -6.697506338400819992, 20.00000000000000000 ) ) ;
#2754 = CIRCLE ( 'NONE', #18706, 4.349999999999976552 ) ;
#2755 = CARTESIAN_POINT ( 'NONE',  ( -20.00000000000000000, -20.00000000000000000, -5.000000000000000000 ) ) ;
#2756 = ORIENTED_EDGE ( 'NONE', *, *, #20592, .F. ) ;
#2757 = VECTOR ( 'NONE', #13947, 1000.000000000000227 ) ;
#2758 = CARTESIAN_POINT ( 'NONE',  ( -19.49999999982360066, -0.1021026942259700004, -2.500000000000000000 ) ) ;
#2759 = VECTOR ( 'NONE', #16812, 1000.000000000000000 ) ;
#2760 = CARTESIAN_POINT ( 'NONE',  ( 118.6002496876800052, -6.405594307115080710, -18.89999999999999858 ) ) ;
#2761 = EDGE_LOOP ( 'NONE', ( #17454, #2076, #20103, #12754 ) ) ;
#2762 = CARTESIAN_POINT ( 'NONE',  ( -62.99678855639989905, 23.76850991288289805, 2.458500000000006569 ) ) ;
#2763 = VECTOR ( 'NONE', #8499, 1000.000000000000114 ) ;
#2764 = CALENDAR_DATE ( 2026, 31, 10 ) ;
#2765 = ORIENTED_EDGE ( 'NONE', *, *, #16902, .T. ) ;
#2766 = ORIENTED_EDGE ( 'NONE', *, *, #6328, .T. ) ;
#2767 = CARTESIAN_POINT ( 'NONE',  ( 114.8905747189831033, 12.63019305843987539, 2.067000000000084103 ) ) ;
#2768 = CARTESIAN_POINT ( 'NONE',  ( -20.00000002229559826, 25.70208919256889857, -8.499999999995555555 ) ) ;
#2769 = ADVANCED_FACE ( 'NONE', ( #22710 ), #19178, .T. ) ;
#2770 = AXIS2_PLACEMENT_3D ( 'NONE', #15058, #6150, #11183 ) ;
#2771 = EDGE_LOOP ( 'NONE', ( #17377, #612, #19152, #6273, #8122 ) ) ;
#2772 = COORDINATED_UNIVERSAL_TIME_OFFSET ( 0, 0, .AHEAD. ) ;
#2773 = AXIS2_PLACEMENT_3D ( 'NONE', #572, #7828, #15177 ) ;
#2774 = DIRECTION ( 'NONE',  ( -6.123237831918399306E-17, 1.569224110909209817E-30, 1.000000000000000000 ) ) ;
#2775 = LOCAL_TIME ( 14, 11, 27.00000000000000000, #17899 ) ;
#2776 = CARTESIAN_POINT ( 'NONE',  ( -26.68881687192900287, -6.639832696913689603, -2.500292893218899692 ) ) ;
#2777 = PERSON_AND_ORGANIZATION ( #2004, #1109 ) ;
#2778 = AXIS2_PLACEMENT_3D ( 'NONE', #6525, #13776, #5103 ) ;
#2779 = CARTESIAN_POINT ( 'NONE',  ( -16.30123784160759826, 29.88528286632680064, -2.500000000000000000 ) ) ;
#2780 = CIRCLE ( 'NONE', #17186, 5.999999999999999112 ) ;
#2781 = EDGE_CURVE ( 'NONE', #16162, #19822, #8604, .T. ) ;
#2782 = DIRECTION ( 'NONE',  ( -6.662161563160872600E-09, 1.000000000000000000, -1.982541115402066096E-15 ) ) ;
#2783 = PERSON_AND_ORGANIZATION ( #11966, #8758 ) ;
#2784 = DIRECTION ( 'NONE',  ( -3.099353312215989243E-62, -9.818186930595456717E-93, 1.000000000000000000 ) ) ;
#2785 = VECTOR ( 'NONE', #12259, 1000.000000000000000 ) ;
#2786 = DIRECTION ( 'NONE',  ( -2.982858504577914959E-17, 2.441916418604795262E-15, 1.000000000000000000 ) ) ;
#2787 = DIRECTION ( 'NONE',  ( 0.000000000000000000, -2.538189087996114879E-14, -1.000000000000000000 ) ) ;
#2788 = APPROVAL_PERSON_ORGANIZATION ( #14298, #11279, #7079 ) ;
#2789 = DIRECTION ( 'NONE',  ( -1.187319687680494078E-16, -2.805478249478275539E-20, -1.000000000000000000 ) ) ;
#2790 = DIRECTION ( 'NONE',  ( 3.356987858687581318E-15, 1.000000000000000000, -5.035481788031372371E-15 ) ) ;
#2791 = APPLICATION_CONTEXT ( 'configuration controlled 3d designs of mechanical parts and assemblies' ) ;
#2792 = CIRCLE ( 'NONE', #5823, 2.500000000000000444 ) ;
#2793 = CARTESIAN_POINT ( 'NONE',  ( -19.99999999999809930, -20.00000000000000000, 8.500000000004551026 ) ) ;
#2794 = ORIENTED_EDGE ( 'NONE', *, *, #5329, .T. ) ;
#2795 = CIRCLE ( 'NONE', #14558, 2.749999999999999112 ) ;
#2796 = ORIENTED_EDGE ( 'NONE', *, *, #675, .T. ) ;
#2797 = CARTESIAN_POINT ( 'NONE',  ( -20.00000000000000000, -20.00000000000000000, -5.000000000000000000 ) ) ;
#2798 = PLANE ( 'NONE',  #14426 ) ;
#2799 = ORIENTED_EDGE ( 'NONE', *, *, #10035, .T. ) ;
#2800 = LINE ( 'NONE', #16922, #6560 ) ;
#2801 = VERTEX_POINT ( 'NONE', #8714 ) ;
#2802 = DIRECTION ( 'NONE',  ( -0.9730401042858023430, 0.2306359803922080620, 5.959266323858944916E-17 ) ) ;
#2803 = CIRCLE ( 'NONE', #19063, 0.09999999999999939493 ) ;
#2804 = APPROVAL_STATUS ( 'not_yet_approved' ) ;
#2805 = CARTESIAN_POINT ( 'NONE',  ( -17.50058776013304396, 23.00629652915649004, -5.000000000000000000 ) ) ;
#2806 = CALENDAR_DATE ( 2026, 31, 10 ) ;
#2807 =( NAMED_UNIT ( * ) PLANE_ANGLE_UNIT ( ) SI_UNIT ( $, .RADIAN. ) );
#2808 = AXIS2_PLACEMENT_3D ( 'NONE', #14494, #21733, #5472 ) ;
#2809 = ADVANCED_FACE ( 'NONE', ( #6343 ), #10163, .T. ) ;
#2810 = CARTESIAN_POINT ( 'NONE',  ( 82.99337969622625621, -17.64642043817426043, 13.00000000000000000 ) ) ;
#2811 = EDGE_CURVE ( 'NONE', #13288, #1580, #21296, .T. ) ;
#2812 = LINE ( 'NONE', #22619, #22671 ) ;
#2813 = DIRECTION ( 'NONE',  ( 0.000000000000000000, 0.000000000000000000, 1.000000000000000000 ) ) ;
#2814 = CARTESIAN_POINT ( 'NONE',  ( 31.45181451370269343, 16.90945435098590011, -21.50000000000000000 ) ) ;
#2815 = EDGE_LOOP ( 'NONE', ( #21014, #18100, #1533, #9477, #3921, #13748 ) ) ;
#2816 = DIRECTION ( 'NONE',  ( 0.000000000000000000, 0.000000000000000000, -1.000000000000000000 ) ) ;
#2817 = FACE_OUTER_BOUND ( 'NONE', #2771, .T. ) ;
#2818 = ORIENTED_EDGE ( 'NONE', *, *, #23140, .F. ) ;
#2819 = DIRECTION ( 'NONE',  ( -0.9730401042858024541, 0.2306359803922080898, 5.959266323853532591E-17 ) ) ;
#2820 = CYLINDRICAL_SURFACE ( 'NONE', #14450, 2.499999999999999112 ) ;
#2821 = ADVANCED_FACE ( 'NONE', ( #3006 ), #17505, .T. ) ;
#2822 = EDGE_CURVE ( 'NONE', #1008, #6050, #7463, .T. ) ;
#2823 = SECURITY_CLASSIFICATION_LEVEL ( 'unclassified' ) ;
#2824 = DIRECTION ( 'NONE',  ( 0.000000000000000000, -1.000000000000000000, 2.081668171172169697E-15 ) ) ;
#2825 = ORIENTED_EDGE ( 'NONE', *, *, #17900, .T. ) ;
#2826 = AXIS2_PLACEMENT_3D ( 'NONE', #1635, #23253, #19580 ) ;
#2827 = EDGE_LOOP ( 'NONE', ( #21305, #11273, #7669, #7385, #180 ) ) ;
#2828 = SHAPE_DEFINITION_REPRESENTATION ( #6827, #1388 ) ;
#2829 = CARTESIAN_POINT ( 'NONE',  ( 30.31182762792540331, -4.706706774123410320, 13.00000000000019895 ) ) ;
#2830 = EDGE_LOOP ( 'NONE', ( #772, #16239, #7465, #14594 ) ) ;
#2831 = PERSON_AND_ORGANIZATION ( #11966, #8758 ) ;
#2832 = PRODUCT ( '1602p_c_16', '1602p_c_16', '', ( #1787 ) ) ;
#2833 = DATE_TIME_ROLE ( 'classification_date' ) ;
#2834 = FACE_OUTER_BOUND ( 'NONE', #6498, .T. ) ;
#2835 = ADVANCED_FACE ( 'NONE', ( #16181, #18330 ), #14176, .T. ) ;
#2836 = FACE_OUTER_BOUND ( 'NONE', #16588, .T. ) ;
#2837 = ORIENTED_EDGE ( 'NONE', *, *, #20360, .F. ) ;
#2838 = CC_DESIGN_PERSON_AND_ORGANIZATION_ASSIGNMENT ( #5220, #2889, ( #5821 ) ) ;
#2839 = PERSON_AND_ORGANIZATION ( #11966, #8758 ) ;
#2840 = CC_DESIGN_PERSON_AND_ORGANIZATION_ASSIGNMENT ( #22205, #15088, ( #10349 ) ) ;
#2841 = ORIENTED_EDGE ( 'NONE', *, *, #3909, .T. ) ;
#2842 = CARTESIAN_POINT ( 'NONE',  ( 28.94448933012489888, 0.3641629059906499877, -13.00000000000039968 ) ) ;
#2843 = LINE ( 'NONE', #21577, #13161 ) ;
#2844 = VERTEX_POINT ( 'NONE', #12401 ) ;
#2845 = EDGE_CURVE ( 'NONE', #16606, #19785, #12025, .T. ) ;
#2846 = EDGE_CURVE ( 'NONE', #11143, #17128, #2047, .T. ) ;
#2847 = LINE ( 'NONE', #17335, #4489 ) ;
#2848 = CARTESIAN_POINT ( 'NONE',  ( -60.04781580374580585, 11.89276268270289982, 5.000000000000000000 ) ) ;
#2849 = LINE ( 'NONE', #19133, #5429 ) ;
#2850 = VERTEX_POINT ( 'NONE', #21761 ) ;
#2851 = VERTEX_POINT ( 'NONE', #5498 ) ;
#2852 = EDGE_CURVE ( 'NONE', #3011, #7550, #2297, .T. ) ;
#2853 = DIRECTION ( 'NONE',  ( 0.2306359803922085339, 0.9730401042858022320, 0.000000000000000000 ) ) ;
#2854 = EDGE_LOOP ( 'NONE', ( #17338, #4452, #20216, #2530, #10256 ) ) ;
#2855 = DATE_AND_TIME ( #10348, #1919 ) ;
#2856 = ADVANCED_BREP_SHAPE_REPRESENTATION ( '', ( #1933, #12739 ), #2264 ) ;
#2857 = VERTEX_POINT ( 'NONE', #7286 ) ;
#2858 = VECTOR ( 'NONE', #1328, 999.9999999999998863 ) ;
#2859 = EDGE_LOOP ( 'NONE', ( #20950, #2722, #2052, #1964 ) ) ;
#2860 = DIRECTION ( 'NONE',  ( -1.000000000000000000, 0.000000000000000000, 0.000000000000000000 ) ) ;
#2861 = COORDINATED_UNIVERSAL_TIME_OFFSET ( 0, 0, .AHEAD. ) ;
#2862 = DIRECTION ( 'NONE',  ( -1.000000000000000000, 0.000000000000000000, 0.000000000000000000 ) ) ;
#2863 = EDGE_CURVE ( 'NONE', #6859, #19990, #14271, .T. ) ;
#2864 = CARTESIAN_POINT ( 'NONE',  ( -26.00000000397469790, 22.95208919201850151, -7.999999999994199307 ) ) ;
#2865 = APPROVAL_ROLE ( '' ) ;
#2866 = AXIS2_PLACEMENT_3D ( 'NONE', #17174, #9947, #13850 ) ;
#2867 = ORIENTED_EDGE ( 'NONE', *, *, #8427, .F. ) ;
#2868 = CARTESIAN_POINT ( 'NONE',  ( -20.00000000000000000, -20.00000000000000000, -5.000000000000000000 ) ) ;
#2869 = FACE_OUTER_BOUND ( 'NONE', #8366, .T. ) ;
#2870 = ORIENTED_EDGE ( 'NONE', *, *, #6668, .F. ) ;
#2871 = EDGE_CURVE ( 'NONE', #5508, #6113, #12853, .T. ) ;
#2872 = EDGE_CURVE ( 'NONE', #14790, #20287, #4872, .T. ) ;
#2873 = CARTESIAN_POINT ( 'NONE',  ( 36.17078849317571354, 12.20740994216783193, -20.00000000000001421 ) ) ;
#2874 = DIRECTION ( 'NONE',  ( -0.9730401042858036753, 0.2306359803922028995, 5.959266323858677443E-17 ) ) ;
#2875 = CYLINDRICAL_SURFACE ( 'NONE', #10354, 2.500000000000000888 ) ;
#2876 = ORIENTED_EDGE ( 'NONE', *, *, #5000, .T. ) ;
#2877 = CARTESIAN_POINT ( 'NONE',  ( -20.00000000000000000, -20.00000000000000000, -2.500000000000000000 ) ) ;
#2878 = PERSON_AND_ORGANIZATION ( #11966, #8758 ) ;
#2879 = PRODUCT_DEFINITION_SHAPE ( 'NONE', 'NONE',  #23490 ) ;
#2880 = EDGE_LOOP ( 'NONE', ( #18097, #579 ) ) ;
#2881 = ORIENTED_EDGE ( 'NONE', *, *, #6692, .T. ) ;
#2882 = PLANE ( 'NONE',  #9235 ) ;
#2883 = PLANE ( 'NONE',  #10029 ) ;
#2884 = VERTEX_POINT ( 'NONE', #14281 ) ;
#2885 = APPROVAL_STATUS ( 'not_yet_approved' ) ;
#2886 = DIRECTION ( 'NONE',  ( -0.005235963827108231460, 0.9999862922474493931, 2.671135040551772162E-18 ) ) ;
#2887 = AXIS2_PLACEMENT_3D ( 'NONE', #17624, #3470, #12631 ) ;
#2888 = PLANE ( 'NONE',  #757 ) ;
#2889 = PERSON_AND_ORGANIZATION_ROLE ( 'classification_officer' ) ;
#2890 = LINE ( 'NONE', #4435, #2178 ) ;
#2891 = VECTOR ( 'NONE', #19827, 1000.000000000000000 ) ;
#2892 = EDGE_CURVE ( 'NONE', #10793, #15994, #7172, .T. ) ;
#2893 = DIRECTION ( 'NONE',  ( -0.005235963827108362431, 0.9999862922474493931, 5.936218956694023463E-19 ) ) ;
#2894 = PERSON_AND_ORGANIZATION_ROLE ( 'design_owner' ) ;
#2895 = CARTESIAN_POINT ( 'NONE',  ( 37.57450334731217367, 9.167194311959766750, 9.000012392934836569 ) ) ;
#2896 = DIRECTION ( 'NONE',  ( 1.000000000000000000, -2.611676738638919574E-15, 0.000000000000000000 ) ) ;
#2897 = ADVANCED_FACE ( 'NONE', ( #1802 ), #5255, .F. ) ;
#2898 = DIRECTION ( 'NONE',  ( -0.9730401042858024541, 0.2306359803922080898, 5.959266323858942451E-17 ) ) ;
#2899 = CARTESIAN_POINT ( 'NONE',  ( 4.267766952966340455, -30.47500000000000142, 20.76776695296636888 ) ) ;
#2900 = ADVANCED_FACE ( 'NONE', ( #12516 ), #9061, .F. ) ;
#2901 = AXIS2_PLACEMENT_3D ( 'NONE', #12, #5608, #14526 ) ;
#2902 = CARTESIAN_POINT ( 'NONE',  ( 2.500000000000000000, 3.061616997868383141E-16, -2.500000000000000000 ) ) ;
#2903 = DIRECTION ( 'NONE',  ( -0.2306359803922027607, -0.9730401042858035643, 1.407521210652529060E-17 ) ) ;
#2904 = ORIENTED_EDGE ( 'NONE', *, *, #18858, .T. ) ;
#2905 = ORIENTED_EDGE ( 'NONE', *, *, #18238, .F. ) ;
#2906 = CARTESIAN_POINT ( 'NONE',  ( -24.86147400983239919, -14.96352599016710094, 2.500000000000000000 ) ) ;
#2907 = CARTESIAN_POINT ( 'NONE',  ( 0.03403376487640590031, -6.499910899608420500, -8.889944397045749129E-14 ) ) ;
#2908 = VERTEX_POINT ( 'NONE', #3478 ) ;
#2909 = CARTESIAN_POINT ( 'NONE',  ( 5.000000000000000000, -31.09999999999999787, 19.00000000000000000 ) ) ;
#2910 = EDGE_LOOP ( 'NONE', ( #18021, #13966 ) ) ;
#2911 = FACE_OUTER_BOUND ( 'NONE', #16737, .T. ) ;
#2912 = DATE_AND_TIME ( #6837, #22097 ) ;
#2913 = DIRECTION ( 'NONE',  ( -6.662160722082822564E-09, 1.000000000000000000, -2.523234146875356491E-15 ) ) ;
#2914 = APPLICATION_CONTEXT ( 'configuration controlled 3d designs of mechanical parts and assemblies' ) ;
#2915 = AXIS2_PLACEMENT_3D ( 'NONE', #6264, #15282, #20739 ) ;
#2916 = DATE_AND_TIME ( #2806, #18674 ) ;
#2917 = VECTOR ( 'NONE', #21359, 999.9999999999998863 ) ;
#2918 = AXIS2_PLACEMENT_3D ( 'NONE', #21630, #12747, #7171 ) ;
#2919 = CARTESIAN_POINT ( 'NONE',  ( -25.49859074735509878, -0.2321374729090470157, 5.000000000000000000 ) ) ;
#2920 = APPROVAL ( #20251, 'UNSPECIFIED' ) ;
#2921 = CARTESIAN_POINT ( 'NONE',  ( -20.00000000000180123, -20.00000000000000000, -7.999999999995458744 ) ) ;
#2922 = DIRECTION ( 'NONE',  ( 1.000000000000000000, 0.000000000000000000, 0.000000000000000000 ) ) ;
#2923 = CYLINDRICAL_SURFACE ( 'NONE', #14940, 1.000000000000000000 ) ;
#2924 = VERTEX_POINT ( 'NONE', #12640 ) ;
#2925 = LINE ( 'NONE', #8739, #21147 ) ;
#2926 = FACE_OUTER_BOUND ( 'NONE', #19641, .T. ) ;
#2927 = ORIENTED_EDGE ( 'NONE', *, *, #18076, .T. ) ;
#2928 = CIRCLE ( 'NONE', #9774, 1.749999999999998668 ) ;
#2929 = CYLINDRICAL_SURFACE ( 'NONE', #12042, 1.749999999999998668 ) ;
#2930 = FACE_BOUND ( 'NONE', #3287, .T. ) ;
#2931 = CONTEXT_DEPENDENT_SHAPE_REPRESENTATION ( #20998, #18813 ) ;
#2932 = CARTESIAN_POINT ( 'NONE',  ( -57.73978104676356793, -25.30277024906009586, -1.339745962155629577 ) ) ;
#2933 = CIRCLE ( 'NONE', #22648, 0.3999999999999982458 ) ;
#2934 = ORIENTED_EDGE ( 'NONE', *, *, #1385, .F. ) ;
#2935 = ORIENTED_EDGE ( 'NONE', *, *, #1595, .T. ) ;
#2936 = APPROVAL_DATE_TIME ( #4485, #12304 ) ;
#2937 = CARTESIAN_POINT ( 'NONE',  ( -22.99999999999959854, -19.33065833018789803, -23.00000000000000000 ) ) ;
#2938 = ADVANCED_FACE ( 'NONE', ( #10753 ), #17985, .T. ) ;
#2939 = EDGE_LOOP ( 'NONE', ( #13738, #7255 ) ) ;
#2940 = DIRECTION ( 'NONE',  ( -0.9999862922474492821, -0.005235963827122071951, 1.187304881134280213E-16 ) ) ;
#2941 = TOROIDAL_SURFACE ( 'NONE', #17356, 3.750000000000000000, 0.5000000000000000000 ) ;
#2942 = APPROVAL_ROLE ( '' ) ;
#2943 = CIRCLE ( 'NONE', #10938, 0.4000000000000010214 ) ;
#2944 = FACE_BOUND ( 'NONE', #9645, .T. ) ;
#2945 = EDGE_CURVE ( 'NONE', #18682, #9640, #14639, .T. ) ;
#2946 = AXIS2_PLACEMENT_3D ( 'NONE', #18008, #11003, #12880 ) ;
#2947 = VECTOR ( 'NONE', #516, 1000.000000000000114 ) ;
#2948 = DIRECTION ( 'NONE',  ( -8.623081276789554834E-17, -1.054188326053478339E-16, -1.000000000000000000 ) ) ;
#2949 = ORIENTED_EDGE ( 'NONE', *, *, #15007, .F. ) ;
#2950 = VERTEX_POINT ( 'NONE', #16291 ) ;
#2951 = AXIS2_PLACEMENT_3D ( 'NONE', #19793, #7212, #3639 ) ;
#2952 = DIRECTION ( 'NONE',  ( 1.138590270679730064E-14, 2.220446049251240387E-15, 1.000000000000000000 ) ) ;
#2953 = CARTESIAN_POINT ( 'NONE',  ( 117.1011158151309957, -12.73035498497280038, 19.59999999999999787 ) ) ;
#2954 = EDGE_LOOP ( 'NONE', ( #14621, #11559 ) ) ;
#2955 = CARTESIAN_POINT ( 'NONE',  ( -60.04781580374580585, 11.89276268270289982, 5.000000000000000000 ) ) ;
#2956 = DIRECTION ( 'NONE',  ( 0.1997366180463827634, 0.8426774492125668203, 0.4999999999999953371 ) ) ;
#2957 = LINE ( 'NONE', #15317, #10391 ) ;
#2958 = AXIS2_PLACEMENT_3D ( 'NONE', #808, #9641, #16855 ) ;
#2959 = EDGE_LOOP ( 'NONE', ( #18310, #3136 ) ) ;
#2960 = ORIENTED_EDGE ( 'NONE', *, *, #11716, .T. ) ;
#2961 = DIRECTION ( 'NONE',  ( -0.005235963827117092427, 0.9999862922474493931, 2.636227439667000721E-16 ) ) ;
#2962 = ORIENTED_EDGE ( 'NONE', *, *, #5087, .T. ) ;
#2963 = APPROVAL_ROLE ( '' ) ;
#2964 = EDGE_CURVE ( 'NONE', #199, #20542, #15031, .T. ) ;
#2965 = EDGE_LOOP ( 'NONE', ( #14831, #5186, #9095, #15766 ) ) ;
#2966 = ORIENTED_EDGE ( 'NONE', *, *, #4909, .T. ) ;
#2967 = CARTESIAN_POINT ( 'NONE',  ( 39.90784330637247024, 24.93874613768021220, -13.00000000000029665 ) ) ;
#2968 = PERSON_AND_ORGANIZATION_ROLE ( 'classification_officer' ) ;
#2969 = CC_DESIGN_DATE_AND_TIME_ASSIGNMENT ( #11996, #2833, ( #8018 ) ) ;
#2970 = CARTESIAN_POINT ( 'NONE',  ( 41.17437060284130013, 11.63805410277980101, -20.00000000000000000 ) ) ;
#2971 = ADVANCED_FACE ( 'NONE', ( #10980, #18201 ), #21013, .F. ) ;
#2972 = EDGE_CURVE ( 'NONE', #19234, #9837, #11896, .T. ) ;
#2973 = LINE ( 'NONE', #8322, #6788 ) ;
#2974 = EDGE_CURVE ( 'NONE', #3517, #17960, #15537, .T. ) ;
#2975 = APPROVAL_DATE_TIME ( #6550, #17427 ) ;
#2976 = AXIS2_PLACEMENT_3D ( 'NONE', #15149, #16828, #8160 ) ;
#2977 = VERTEX_POINT ( 'NONE', #8303 ) ;
#2978 = DIRECTION ( 'NONE',  ( 0.9730401042858036753, -0.2306359803922028995, -5.432877459303547669E-17 ) ) ;
#2979 = CARTESIAN_POINT ( 'NONE',  ( 39.74442752440959481, 5.605205456207779768, -20.00000000000000000 ) ) ;
#2980 = ORIENTED_EDGE ( 'NONE', *, *, #2863, .F. ) ;
#2981 = DIRECTION ( 'NONE',  ( 0.9730401042858035643, -0.2306359803922028717, -5.958148513035547083E-17 ) ) ;
#2982 = CARTESIAN_POINT ( 'NONE',  ( -69.90454993788389970, 6.134066389561166233, -3.000000000000079936 ) ) ;
#2983 = CARTESIAN_POINT ( 'NONE',  ( -23.50000000000000000, -19.99999999999999289, 5.000000000000000000 ) ) ;
#2984 = ORIENTED_EDGE ( 'NONE', *, *, #8508, .F. ) ;
#2985 = CARTESIAN_POINT ( 'NONE',  ( -26.72214353971689960, -0.1399180949200579949, 2.500999999999910184 ) ) ;
#2986 = DATE_TIME_ROLE ( 'creation_date' ) ;
#2987 = ADVANCED_FACE ( 'NONE', ( #10103 ), #16522, .T. ) ;
#2988 = ORIENTED_EDGE ( 'NONE', *, *, #15770, .F. ) ;
#2989 = VERTEX_POINT ( 'NONE', #12973 ) ;
#2990 = DIRECTION ( 'NONE',  ( -0.9730401042858036753, 0.2306359803922028995, -2.804983810440358801E-16 ) ) ;
#2991 = LINE ( 'NONE', #17484, #7349 ) ;
#2992 = CARTESIAN_POINT ( 'NONE',  ( 6.500000000000000000, -17.30000000000000071, -2.500000000000000000 ) ) ;
#2993 = CALENDAR_DATE ( 2026, 31, 10 ) ;
#2994 = DIRECTION ( 'NONE',  ( -6.662111519016958720E-09, 1.000000000000000000, -2.523234146875356491E-15 ) ) ;
#2995 = APPROVAL ( #5672, 'UNSPECIFIED' ) ;
#2996 = PRODUCT_RELATED_PRODUCT_CATEGORY ( 'detail', '', ( #4919 ) ) ;
#2997 = DIRECTION ( 'NONE',  ( 0.9730401042858036753, -0.2306359803922031493, 2.740969466505752002E-16 ) ) ;
#2998 = CYLINDRICAL_SURFACE ( 'NONE', #1013, 3.499999999999999556 ) ;
#2999 = EDGE_CURVE ( 'NONE', #134, #13843, #19212, .T. ) ;
#3000 = EDGE_CURVE ( 'NONE', #7633, #18172, #9992, .T. ) ;
#3001 = AXIS2_PLACEMENT_3D ( 'NONE', #10521, #10171, #23313 ) ;
#3002 = CARTESIAN_POINT ( 'NONE',  ( 2.499999999999970246, -28.60000000000000142, 21.50000000000000000 ) ) ;
#3003 = APPLICATION_PROTOCOL_DEFINITION ( 'international standard', 'config_control_design', 1994, #2914 ) ;
#3004 = CARTESIAN_POINT ( 'NONE',  ( 37.11020026392842652, 8.343731908207489667, 8.942923417076606540 ) ) ;
#3005 = DIRECTION ( 'NONE',  ( -0.9730401042858035643, 0.2306359803922028717, 5.959266323858677443E-17 ) ) ;
#3006 = FACE_OUTER_BOUND ( 'NONE', #228, .T. ) ;
#3007 = DIRECTION ( 'NONE',  ( 0.9999862922474493931, 0.005235963827117055998, -1.750845403988397166E-31 ) ) ;
#3008 = DIRECTION ( 'NONE',  ( -0.2306359803922028440, -0.9730401042858034533, -4.307366329831518561E-32 ) ) ;
#3009 = VERTEX_POINT ( 'NONE', #691 ) ;
#3010 = DIRECTION ( 'NONE',  ( -0.6880432561069586006, 0.1630842657209347069, -0.7071067811865459074 ) ) ;
#3011 = VERTEX_POINT ( 'NONE', #1037 ) ;
#3012 = EDGE_CURVE ( 'NONE', #5266, #6885, #22773, .T. ) ;
#3013 = PRODUCT ( 'BR-Y-121', 'BR-Y-121', '', ( #12536 ) ) ;
#3014 = ORIENTED_EDGE ( 'NONE', *, *, #17997, .F. ) ;
#3015 = CARTESIAN_POINT ( 'NONE',  ( 37.56481403710107969, 24.44795204016911327, -12.00000000000050271 ) ) ;
#3016 = DIRECTION ( 'NONE',  ( -0.9080662505692100872, 0.4188265566761218417, -1.040834085574018826E-15 ) ) ;
#3017 = LOCAL_TIME ( 14, 11, 27.00000000000000000, #12478 ) ;
#3018 = VERTEX_POINT ( 'NONE', #6521 ) ;
#3019 = CONICAL_SURFACE ( 'NONE', #22331, 2.283500000000000529, 0.7853981633974419507 ) ;
#3020 = PLANE ( 'NONE',  #13390 ) ;
#3021 = EDGE_CURVE ( 'NONE', #21452, #9837, #19594, .T. ) ;
#3022 = ORIENTED_EDGE ( 'NONE', *, *, #2999, .T. ) ;
#3023 = DIRECTION ( 'NONE',  ( -0.9999862922474492821, -0.005235963827121951387, 1.187304881134294758E-16 ) ) ;
#3024 = COORDINATED_UNIVERSAL_TIME_OFFSET ( 0, 0, .AHEAD. ) ;
#3025 = LINE ( 'NONE', #17170, #998 ) ;
#3026 = EDGE_CURVE ( 'NONE', #7364, #10083, #21102, .T. ) ;
#3027 = ADVANCED_FACE ( 'NONE', ( #18886 ), #20223, .T. ) ;
#3028 = PERSON_AND_ORGANIZATION_ROLE ( 'classification_officer' ) ;
#3029 = DIRECTION ( 'NONE',  ( 1.000000000000000000, 1.304396158928280155E-15, 0.000000000000000000 ) ) ;
#3030 = LINE ( 'NONE', #10535, #2196 ) ;
#3031 = DIRECTION ( 'NONE',  ( 1.000000000000000000, 0.000000000000000000, 0.000000000000000000 ) ) ;
#3032 = VECTOR ( 'NONE', #9818, 1000.000000000000227 ) ;
#3033 =( GEOMETRIC_REPRESENTATION_CONTEXT ( 3 ) GLOBAL_UNCERTAINTY_ASSIGNED_CONTEXT ( ( #3484 ) ) GLOBAL_UNIT_ASSIGNED_CONTEXT ( ( #6065, #16141, #14246 ) ) REPRESENTATION_CONTEXT ( 'NONE', 'WORKASPACE' ) );
#3034 = CARTESIAN_POINT ( 'NONE',  ( 120.2377651484647032, 0.5029904333151811180, 13.00000000000000000 ) ) ;
#3035 = CIRCLE ( 'NONE', #4939, 5.000000000000000888 ) ;
#3036 = EDGE_LOOP ( 'NONE', ( #22668, #10904, #8497, #7070 ) ) ;
#3037 = PLANE ( 'NONE',  #18126 ) ;
#3038 = DESIGN_CONTEXT ( 'detailed design', #7768, 'design' ) ;
#3039 = CARTESIAN_POINT ( 'NONE',  ( 31.14187293219668717, -1.979315439058177528, -11.00000000000039613 ) ) ;
#3040 = ORIENTED_EDGE ( 'NONE', *, *, #15651, .F. ) ;
#3041 = CARTESIAN_POINT ( 'NONE',  ( 33.65824643301471042, 10.51177500877083659, -8.996924156394149108 ) ) ;
#3042 = CARTESIAN_POINT ( 'NONE',  ( -3.458317987535629801, 19.03127855354509990, -7.892745253163399067E-16 ) ) ;
#3043 = AXIS2_PLACEMENT_3D ( 'NONE', #12399, #19630, #3355 ) ;
#3044 = EDGE_LOOP ( 'NONE', ( #13952, #10936, #14151, #1665 ) ) ;
#3045 = APPROVAL_DATE_TIME ( #8637, #13695 ) ;
#3046 = DIRECTION ( 'NONE',  ( 6.124378941433959925E-17, 0.000000000000000000, 1.000000000000000000 ) ) ;
#3047 = AXIS2_PLACEMENT_3D ( 'NONE', #1908, #18554, #2145 ) ;
#3048 = VERTEX_POINT ( 'NONE', #20654 ) ;
#3049 = ORIENTED_EDGE ( 'NONE', *, *, #14612, .F. ) ;
#3050 = APPLICATION_CONTEXT ( 'configuration controlled 3d designs of mechanical parts and assemblies' ) ;
#3051 = PRODUCT_DEFINITION ( 'UNKNOWN', '', #4225, #23214 ) ;
#3052 = DATE_AND_TIME ( #12105, #14480 ) ;
#3053 = LINE ( 'NONE', #19791, #14108 ) ;
#3054 = ADVANCED_FACE ( 'NONE', ( #7520 ), #15313, .T. ) ;
#3055 = ORIENTED_EDGE ( 'NONE', *, *, #22538, .F. ) ;
#3056 = LOCAL_TIME ( 14, 11, 27.00000000000000000, #12497 ) ;
#3057 = DIRECTION ( 'NONE',  ( -0.9730401042858036753, 0.2306359803922028995, 5.959266323858677443E-17 ) ) ;
#3058 = AXIS2_PLACEMENT_3D ( 'NONE', #14078, #9629, #2922 ) ;
#3059 = COORDINATED_UNIVERSAL_TIME_OFFSET ( 0, 0, .AHEAD. ) ;
#3060 = PERSON_AND_ORGANIZATION ( #17283, #6886 ) ;
#3061 = CARTESIAN_POINT ( 'NONE',  ( 26.11627841292215280, -8.532812502301741375, -20.00000000000000000 ) ) ;
#3062 = AXIS2_PLACEMENT_3D ( 'NONE', #12486, #14369, #18055 ) ;
#3063 = CARTESIAN_POINT ( 'NONE',  ( 37.37362508103680625, 25.08661566644150298, -13.00000000000049916 ) ) ;
#3064 = ORIENTED_EDGE ( 'NONE', *, *, #3188, .F. ) ;
#3065 = EDGE_CURVE ( 'NONE', #22508, #12435, #7102, .T. ) ;
#3066 = LOCAL_TIME ( 14, 11, 27.00000000000000000, #4893 ) ;
#3067 = ORIENTED_EDGE ( 'NONE', *, *, #18695, .T. ) ;
#3068 = LOCAL_TIME ( 14, 11, 27.00000000000000000, #15009 ) ;
#3069 = CARTESIAN_POINT ( 'NONE',  ( -19.88588018851017480, 25.44948316784238074, 5.000000000004453327 ) ) ;
#3070 = CARTESIAN_POINT ( 'NONE',  ( -16.50000000202540207, 1.899127378699219992, 8.000000000004471090 ) ) ;
#3071 = ORIENTED_EDGE ( 'NONE', *, *, #1827, .T. ) ;
#3072 = CONICAL_SURFACE ( 'NONE', #16340, 2.283500000000000529, 0.7853981633974539411 ) ;
#3073 = DIRECTION ( 'NONE',  ( -0.9997651245880592175, -0.02167246311387461058, 0.000000000000000000 ) ) ;
#3074 = DIRECTION ( 'NONE',  ( 6.052506032659479608E-17, 4.865024487662030352E-15, 1.000000000000000000 ) ) ;
#3075 = DIRECTION ( 'NONE',  ( -0.9730401042858036753, 0.2306359803922031493, 5.432877459303543355E-17 ) ) ;
#3076 = EDGE_LOOP ( 'NONE', ( #22913, #12364, #4860, #11218, #15084 ) ) ;
#3077 = ORIENTED_EDGE ( 'NONE', *, *, #21436, .T. ) ;
#3078 = DIRECTION ( 'NONE',  ( -1.000000000000000000, -6.662112528310618598E-09, 2.269018306577664942E-13 ) ) ;
#3079 = VERTEX_POINT ( 'NONE', #4389 ) ;
#3080 = VECTOR ( 'NONE', #20475, 1000.000000000000114 ) ;
#3081 = SHAPE_DEFINITION_REPRESENTATION ( #12139, #11914 ) ;
#3082 = ORIENTED_EDGE ( 'NONE', *, *, #8388, .F. ) ;
#3083 = ORIENTED_EDGE ( 'NONE', *, *, #2407, .T. ) ;
#3084 = CARTESIAN_POINT ( 'NONE',  ( 35.84667945578129888, -10.83917230622230043, -13.00000000000000000 ) ) ;
#3085 = DATE_AND_TIME ( #3208, #19430 ) ;
#3086 = CC_DESIGN_APPROVAL ( #1680, ( #4578 ) ) ;
#3087 = FACE_OUTER_BOUND ( 'NONE', #3044, .T. ) ;
#3088 = CC_DESIGN_APPROVAL ( #1159, ( #3463 ) ) ;
#3089 = TOROIDAL_SURFACE ( 'NONE', #14850, 2.600000000000000089, 0.1000000000000000056 ) ;
#3090 = SHAPE_REPRESENTATION_RELATIONSHIP ( 'NONE' , 'NONE' ,  #8415, #22945 ) ;
#3091 = DIRECTION ( 'NONE',  ( -3.099353312215988811E-62, -9.818186930595456717E-93, 1.000000000000000000 ) ) ;
#3092 =( REPRESENTATION_RELATIONSHIP ('NONE','NONE', #18771, #7508 ) REPRESENTATION_RELATIONSHIP_WITH_TRANSFORMATION ( #8350 )SHAPE_REPRESENTATION_RELATIONSHIP( ) );
#3093 = LINE ( 'NONE', #6786, #17574 ) ;
#3094 = ADVANCED_FACE ( 'NONE', ( #18449, #9860 ), #18997, .F. ) ;
#3095 = PERSON_AND_ORGANIZATION ( #11966, #8758 ) ;
#3096 = ORIENTED_EDGE ( 'NONE', *, *, #19547, .F. ) ;
#3097 = CARTESIAN_POINT ( 'NONE',  ( -20.00000000397369959, 22.95208919256949898, -2.500000000000059952 ) ) ;
#3098 = DIRECTION ( 'NONE',  ( 1.138590270679734009E-14, 2.220446049251240387E-15, 1.000000000000000000 ) ) ;
#3099 = ORIENTED_EDGE ( 'NONE', *, *, #10881, .F. ) ;
#3100 = LOCAL_TIME ( 14, 11, 27.00000000000000000, #4194 ) ;
#3101 = CARTESIAN_POINT ( 'NONE',  ( -25.29411765129429668, 25.77561860384869874, -6.749999999994369837 ) ) ;
#3102 = FACE_OUTER_BOUND ( 'NONE', #2830, .T. ) ;
#3103 = ORIENTED_EDGE ( 'NONE', *, *, #22094, .T. ) ;
#3104 = DIRECTION ( 'NONE',  ( 6.123237831918399306E-17, -1.569224110909209817E-30, -1.000000000000000000 ) ) ;
#3105 = CONICAL_SURFACE ( 'NONE', #12614, 5.386751345948120218, 1.047197551196598297 ) ;
#3106 = ADVANCED_FACE ( 'NONE', ( #22543 ), #23003, .T. ) ;
#3107 = EDGE_CURVE ( 'NONE', #9845, #8168, #8188, .T. ) ;
#3108 = PERSON_AND_ORGANIZATION_ROLE ( 'design_supplier' ) ;
#3109 = ORIENTED_EDGE ( 'NONE', *, *, #14116, .T. ) ;
#3110 = EDGE_LOOP ( 'NONE', ( #6015, #12221, #8373, #9509 ) ) ;
#3111 = CARTESIAN_POINT ( 'NONE',  ( -66.39991637198865249, -25.34811502593582944, 3.660254037844372199 ) ) ;
#3112 = ORGANIZATION ( 'NAUO-ORG25', 'UNSPECIFIED', 'UNSPECIFIED' ) ;
#3113 = LINE ( 'NONE', #14266, #3477 ) ;
#3114 = DATE_AND_TIME ( #2993, #19786 ) ;
#3115 = PLANE ( 'NONE',  #11538 ) ;
#3116 = CARTESIAN_POINT ( 'NONE',  ( 34.67470932959380292, 24.53963568513870186, 15.00000000000000000 ) ) ;
#3117 = CARTESIAN_POINT ( 'NONE',  ( -26.00000000397409750, 22.95208919201850151, -5.499999999994199307 ) ) ;
#3118 = LOCAL_TIME ( 14, 11, 27.00000000000000000, #9048 ) ;
#3119 = DIRECTION ( 'NONE',  ( 1.000000000000000000, 0.000000000000000000, 0.000000000000000000 ) ) ;
#3120 = AXIS2_PLACEMENT_3D ( 'NONE', #5126, #12381, #17830 ) ;
#3121 = PERSON ( 'NAUO-PER25', 'UNSPECIFIED', 'UNSPECIFIED', ('UNSPECIFIED'), ('UNSPECIFIED'), ('UNSPECIFIED') ) ;
#3122 = VECTOR ( 'NONE', #19411, 1000.000000000000000 ) ;
#3123 = DIRECTION ( 'NONE',  ( 2.269747459788999852E-13, 2.220446049250325308E-15, 1.000000000000000000 ) ) ;
#3124 = EDGE_CURVE ( 'NONE', #4115, #10804, #2843, .T. ) ;
#3125 = APPROVAL_ROLE ( '' ) ;
#3126 = CONICAL_SURFACE ( 'NONE', #1588, 2.624999999999998668, 0.4636476090008101458 ) ;
#3127 = CC_DESIGN_SECURITY_CLASSIFICATION ( #10735, ( #23507 ) ) ;
#3128 = CARTESIAN_POINT ( 'NONE',  ( 36.05798491156198082, 7.755984563572242863, 8.806404184311324101 ) ) ;
#3129 = DIRECTION ( 'NONE',  ( -0.9730401042858022320, 0.2306359803922080343, 1.587386801403055476E-31 ) ) ;
#3130 = CC_DESIGN_DATE_AND_TIME_ASSIGNMENT ( #21801, #20146, ( #4302 ) ) ;
#3131 = AXIS2_PLACEMENT_3D ( 'NONE', #10630, #8847, #16079 ) ;
#3132 = DIRECTION ( 'NONE',  ( -0.9730401042858036753, 0.2306359803922031493, -2.804983810440361760E-16 ) ) ;
#3133 = DIRECTION ( 'NONE',  ( 7.252994924361790472E-16, -5.047364287626240282E-15, -1.000000000000000000 ) ) ;
#3134 = APPROVAL ( #5083, 'UNSPECIFIED' ) ;
#3135 = CARTESIAN_POINT ( 'NONE',  ( 36.10037903421270755, -9.768828191507889613, -3.399999999999939959 ) ) ;
#3136 = ORIENTED_EDGE ( 'NONE', *, *, #8962, .F. ) ;
#3137 = AXIS2_PLACEMENT_3D ( 'NONE', #9621, #12924, #14949 ) ;
#3138 = DIRECTION ( 'NONE',  ( -0.9730401042858036753, 0.2306359803922031493, -2.804983810440356829E-16 ) ) ;
#3139 = ADVANCED_FACE ( 'NONE', ( #15889 ), #4969, .T. ) ;
#3140 = ADVANCED_FACE ( 'NONE', ( #13994 ), #17572, .F. ) ;
#3141 = LOCAL_TIME ( 14, 11, 27.00000000000000000, #3059 ) ;
#3142 = CC_DESIGN_DATE_AND_TIME_ASSIGNMENT ( #11544, #13523, ( #19033 ) ) ;
#3143 = VERTEX_POINT ( 'NONE', #21227 ) ;
#3144 = CARTESIAN_POINT ( 'NONE',  ( -13.66075527208050033, 1.277470069177119916, -2.500000000000000000 ) ) ;
#3145 = VERTEX_POINT ( 'NONE', #17917 ) ;
#3146 = VECTOR ( 'NONE', #15542, 999.9999999999998863 ) ;
#3147 = AXIS2_PLACEMENT_3D ( 'NONE', #20459, #9427, #6088 ) ;
#3148 = LINE ( 'NONE', #1463, #5415 ) ;
#3149 = ADVANCED_BREP_SHAPE_REPRESENTATION ( '', ( #9741, #12739 ), #21969 ) ;
#3150 = ORIENTED_EDGE ( 'NONE', *, *, #13119, .T. ) ;
#3151 = VECTOR ( 'NONE', #21306, 1000.000000000000000 ) ;
#3152 = CARTESIAN_POINT ( 'NONE',  ( 39.67523673029189979, 5.313293424921970320, 15.90000000000000036 ) ) ;
#3153 = SHAPE_DEFINITION_REPRESENTATION ( #13679, #17646 ) ;
#3154 = DIRECTION ( 'NONE',  ( 2.982858504577914959E-17, -2.441916418604795262E-15, -1.000000000000000000 ) ) ;
#3155 = APPROVAL_ROLE ( '' ) ;
#3156 = CARTESIAN_POINT ( 'NONE',  ( 0.000000000000000000, 0.000000000000000000, 0.000000000000000000 ) ) ;
#3158 = DIRECTION ( 'NONE',  ( -2.269700743865584947E-13, -2.220446049247695246E-15, -1.000000000000000000 ) ) ;
#3157 = VECTOR ( 'NONE', #9745, 1000.000000000000000 ) ;
#3159 = LINE ( 'NONE', #10428, #16604 ) ;
#3160 = EDGE_CURVE ( 'NONE', #17030, #17831, #19985, .T. ) ;
#3161 = CC_DESIGN_APPROVAL ( #347, ( #2395 ) ) ;
#3162 = CARTESIAN_POINT ( 'NONE',  ( -31.64676348097539815, 7.334526001134540785, 3.750000000000000000 ) ) ;
#3163 = AXIS2_PLACEMENT_3D ( 'NONE', #527, #18477, #15127 ) ;
#3164 = EDGE_LOOP ( 'NONE', ( #330, #12431, #18994, #2642 ) ) ;
#3165 = DIRECTION ( 'NONE',  ( 0.005235963827108352890, -0.9999862922474493931, -2.671135040551771006E-18 ) ) ;
#3166 = VECTOR ( 'NONE', #14996, 1000.000000000000227 ) ;
#3167 = CARTESIAN_POINT ( 'NONE',  ( 32.96699026062352544, 10.39752682851222865, -26.30000000000050520 ) ) ;
#3168 = VERTEX_POINT ( 'NONE', #1631 ) ;
#3169 = CARTESIAN_POINT ( 'NONE',  ( 33.53333525001635707, 9.983743838774772783, -8.996869837679783544 ) ) ;
#3170 = CARTESIAN_POINT ( 'NONE',  ( 2.500000000000000000, -28.60000000000000142, -19.00000000000000000 ) ) ;
#3171 = EDGE_CURVE ( 'NONE', #4894, #8501, #4853, .T. ) ;
#3173 = ORIENTED_EDGE ( 'NONE', *, *, #5711, .F. ) ;
#3172 = ADVANCED_FACE ( 'NONE', ( #8901 ), #11674, .F. ) ;
#3174 = DATE_AND_TIME ( #8882, #10304 ) ;
#3175 = CARTESIAN_POINT ( 'NONE',  ( 5.000000000000000000, -28.60000000000000142, 6.250000000000000000 ) ) ;
#3176 = VERTEX_POINT ( 'NONE', #19338 ) ;
#3177 = CIRCLE ( 'NONE', #16432, 4.250000000000000000 ) ;
#3178 = ORIENTED_EDGE ( 'NONE', *, *, #21632, .F. ) ;
#3179 = PERSON_AND_ORGANIZATION ( #11966, #8758 ) ;
#3180 = DIRECTION ( 'NONE',  ( 0.9730401042858035643, -0.2306359803922028717, -5.432877459303547053E-17 ) ) ;
#3181 = VECTOR ( 'NONE', #11999, 1000.000000000000114 ) ;
#3182 = ORIENTED_EDGE ( 'NONE', *, *, #12741, .F. ) ;
#3183 = DIRECTION ( 'NONE',  ( -0.005235964026270697493, 0.9999862922464064496, -2.442051063555178886E-15 ) ) ;
#3184 = CALENDAR_DATE ( 2026, 31, 10 ) ;
#3185 = CIRCLE ( 'NONE', #6222, 6.499999999999997335 ) ;
#3186 = CALENDAR_DATE ( 2026, 31, 10 ) ;
#3187 = CARTESIAN_POINT ( 'NONE',  ( 120.8143550994449953, 2.935590694028619829, -13.00000000000000000 ) ) ;
#3188 = EDGE_CURVE ( 'NONE', #7380, #20922, #12577, .T. ) ;
#3189 = DIRECTION ( 'NONE',  ( 0.000000000000000000, -1.000000000000000000, 2.081668171172169697E-15 ) ) ;
#3190 = ORIENTED_EDGE ( 'NONE', *, *, #10159, .T. ) ;
#3191 = AXIS2_PLACEMENT_3D ( 'NONE', #6484, #21084, #11977 ) ;
#3192 = ORIENTED_EDGE ( 'NONE', *, *, #21762, .F. ) ;
#3193 = EDGE_CURVE ( 'NONE', #17928, #13217, #16240, .T. ) ;
#3194 = DIRECTION ( 'NONE',  ( -0.2306359803922085339, -0.9730401042858022320, 0.000000000000000000 ) ) ;
#3195 = CARTESIAN_POINT ( 'NONE',  ( -68.69007546624879978, 8.433449002107520798, 2.873144230283079984E-15 ) ) ;
#3196 = VERTEX_POINT ( 'NONE', #19811 ) ;
#3197 = ADVANCED_FACE ( 'NONE', ( #16126 ), #1288, .T. ) ;
#3198 = FACE_BOUND ( 'NONE', #22784, .T. ) ;
#3199 = DIRECTION ( 'NONE',  ( -0.9730401042858036753, 0.2306359803922031493, 5.432877459303543355E-17 ) ) ;
#3200 = ORIENTED_EDGE ( 'NONE', *, *, #1810, .F. ) ;
#3201 = VERTEX_POINT ( 'NONE', #5099 ) ;
#3202 = CARTESIAN_POINT ( 'NONE',  ( 37.91003399039541222, 9.225896048119828663, -29.25000000000049738 ) ) ;
#3203 = ORIENTED_EDGE ( 'NONE', *, *, #19668, .T. ) ;
#3204 = PERSON_AND_ORGANIZATION_ROLE ( 'design_supplier' ) ;
#3205 = ORIENTED_EDGE ( 'NONE', *, *, #12997, .F. ) ;
#3206 = VERTEX_POINT ( 'NONE', #17442 ) ;
#3207 = CYLINDRICAL_SURFACE ( 'NONE', #9593, 4.250000000000000000 ) ;
#3208 = CALENDAR_DATE ( 2026, 31, 10 ) ;
#3209 = DIRECTION ( 'NONE',  ( -0.005235963827110212514, 0.9999862922474493931, -1.836993535195700665E-15 ) ) ;
#3210 =( LENGTH_UNIT ( ) NAMED_UNIT ( * ) SI_UNIT ( .MILLI., .METRE. ) );
#3211 = CARTESIAN_POINT ( 'NONE',  ( -17.00058718854806017, -0.04792152746387602635, 5.000000000000000000 ) ) ;
#3212 = CC_DESIGN_PERSON_AND_ORGANIZATION_ASSIGNMENT ( #15245, #22488, ( #7616 ) ) ;
#3213 = APPROVAL_STATUS ( 'not_yet_approved' ) ;
#3214 = PRODUCT_DEFINITION_SHAPE ( 'NONE', 'NONE',  #8957 ) ;
#3215 = ORIENTED_EDGE ( 'NONE', *, *, #13792, .T. ) ;
#3216 = DIRECTION ( 'NONE',  ( 0.7071067811865475727, 0.000000000000000000, -0.7071067811865474617 ) ) ;
#3217 = DIRECTION ( 'NONE',  ( -0.9730401042858035643, 0.2306359803922028717, 5.667427308550587516E-17 ) ) ;
#3218 = ORIENTED_EDGE ( 'NONE', *, *, #4848, .F. ) ;
#3219 = DIRECTION ( 'NONE',  ( 2.269747459789000104E-13, 2.220446049250330436E-15, 1.000000000000000000 ) ) ;
#3220 = VECTOR ( 'NONE', #22894, 1000.000000000000000 ) ;
#3221 = CARTESIAN_POINT ( 'NONE',  ( 34.67470932959380292, 24.53963568513870186, 11.00000000000000000 ) ) ;
#3222 = DIRECTION ( 'NONE',  ( -3.099353312215989243E-62, -9.818186930595456717E-93, 1.000000000000000000 ) ) ;
#3223 = ORIENTED_EDGE ( 'NONE', *, *, #5299, .T. ) ;
#3224 = DIRECTION ( 'NONE',  ( 0.000000000000000000, 0.000000000000000000, 1.000000000000000000 ) ) ;
#3225 = APPROVAL_DATE_TIME ( #21265, #5465 ) ;
#3226 = VERTEX_POINT ( 'NONE', #17689 ) ;
#3227 = ORIENTED_EDGE ( 'NONE', *, *, #14039, .F. ) ;
#3228 = FACE_OUTER_BOUND ( 'NONE', #22880, .T. ) ;
#3229 = CARTESIAN_POINT ( 'NONE',  ( 35.59419854219520118, 9.774809681453270116, -29.25000000000050093 ) ) ;
#3230 = FACE_OUTER_BOUND ( 'NONE', #7963, .T. ) ;
#3231 = CALENDAR_DATE ( 2026, 31, 10 ) ;
#3232 = DIRECTION ( 'NONE',  ( -0.9997651245102161521, -0.02167246670483386276, 0.000000000000000000 ) ) ;
#3233 = EDGE_CURVE ( 'NONE', #11903, #4956, #8773, .T. ) ;
#3234 = DIRECTION ( 'NONE',  ( 6.123230159571619958E-17, 0.000000000000000000, 1.000000000000000000 ) ) ;
#3235 = AXIS2_PLACEMENT_3D ( 'NONE', #13284, #7587, #13065 ) ;
#3236 = CARTESIAN_POINT ( 'NONE',  ( 0.000000000000000000, 0.000000000000000000, 0.000000000000000000 ) ) ;
#3237 = EDGE_CURVE ( 'NONE', #22084, #11858, #4052, .T. ) ;
#3238 = EDGE_CURVE ( 'NONE', #20234, #8857, #1506, .T. ) ;
#3239 = ORIENTED_EDGE ( 'NONE', *, *, #369, .F. ) ;
#3240 = DIRECTION ( 'NONE',  ( 0.005235963827102643048, -0.9999862922474495042, -7.724582913192744961E-15 ) ) ;
#3241 = APPLICATION_PROTOCOL_DEFINITION ( 'international standard', 'config_control_design', 1994, #21695 ) ;
#3242 = CARTESIAN_POINT ( 'NONE',  ( 36.33223090203711791, 11.71027499018234153, 8.762640180330951267 ) ) ;
#3243 = LINE ( 'NONE', #10509, #9359 ) ;
#3244 = DIRECTION ( 'NONE',  ( -0.9730401042858024541, 0.2306359803922080898, 5.959266323858942451E-17 ) ) ;
#3245 = DIRECTION ( 'NONE',  ( -4.302370362259564196E-33, 3.446306084657139973E-17, 1.000000000000000000 ) ) ;
#3246 = LINE ( 'NONE', #19405, #9580 ) ;
#3247 = EDGE_LOOP ( 'NONE', ( #13344, #13513, #21944, #8145 ) ) ;
#3248 = DIRECTION ( 'NONE',  ( 0.000000000000000000, -1.000000000000000000, 1.954868129030600086E-15 ) ) ;
#3249 = UNCERTAINTY_MEASURE_WITH_UNIT (LENGTH_MEASURE( 1.000000000000000082E-05 ), #8484, 'distance_accuracy_value', 'NONE');
#3250 = AXIS2_PLACEMENT_3D ( 'NONE', #5428, #17790, #21566 ) ;
#3251 = ORIENTED_EDGE ( 'NONE', *, *, #10708, .T. ) ;
#3252 = DIRECTION ( 'NONE',  ( -1.227507208848341976E-15, -4.920447605136010024E-15, -1.000000000000000000 ) ) ;
#3253 = DIRECTION ( 'NONE',  ( -0.9730401042858035643, 0.2306359803922028717, -2.804983810440358308E-16 ) ) ;
#3254 = VERTEX_POINT ( 'NONE', #10338 ) ;
#3255 = DIRECTION ( 'NONE',  ( -0.9286452767786568252, -1.871119812896369614E-17, -0.3709689338970204586 ) ) ;
#3256 = CIRCLE ( 'NONE', #20326, 5.000000000000000888 ) ;
#3257 = ADVANCED_FACE ( 'NONE', ( #15780, #23007 ), #3304, .F. ) ;
#3258 = EDGE_LOOP ( 'NONE', ( #3452, #11458 ) ) ;
#3259 = PLANE ( 'NONE',  #8723 ) ;
#3260 = SECURITY_CLASSIFICATION_LEVEL ( 'unclassified' ) ;
#3261 = DIRECTION ( 'NONE',  ( -0.9999862922474493931, -0.005235963827108420544, 0.000000000000000000 ) ) ;
#3262 = CC_DESIGN_DATE_AND_TIME_ASSIGNMENT ( #15300, #16847, ( #1928 ) ) ;
#3263 = CC_DESIGN_PERSON_AND_ORGANIZATION_ASSIGNMENT ( #7050, #17379, ( #795 ) ) ;
#3264 =( NAMED_UNIT ( * ) PLANE_ANGLE_UNIT ( ) SI_UNIT ( $, .RADIAN. ) );
#3265 = CARTESIAN_POINT ( 'NONE',  ( 118.5079952955230027, -6.794810348829390279, 15.90000000000000036 ) ) ;
#3266 = ADVANCED_FACE ( 'NONE', ( #14113, #12463, #19692, #22903 ), #23356, .F. ) ;
#3267 = ADVANCED_FACE ( 'NONE', ( #7691 ), #21815, .F. ) ;
#3268 = CARTESIAN_POINT ( 'NONE',  ( 35.09747506357100377, 11.43410645592859964, 27.68999999999999773 ) ) ;
#3269 = APPLICATION_PROTOCOL_DEFINITION ( 'international standard', 'config_control_design', 1994, #19158 ) ;
#3270 =( GEOMETRIC_REPRESENTATION_CONTEXT ( 3 ) GLOBAL_UNCERTAINTY_ASSIGNED_CONTEXT ( ( #14645 ) ) GLOBAL_UNIT_ASSIGNED_CONTEXT ( ( #20005, #6972, #14072 ) ) REPRESENTATION_CONTEXT ( 'NONE', 'WORKASPACE' ) );
#3271 = DIRECTION ( 'NONE',  ( -0.9999862922474493931, -0.005235963827110273229, -0.000000000000000000 ) ) ;
#3272 = VERTEX_POINT ( 'NONE', #3888 ) ;
#3273 = CARTESIAN_POINT ( 'NONE',  ( 37.46113131852679601, -4.027891576221660053, -20.00000000000000000 ) ) ;
#3274 = AXIS2_PLACEMENT_3D ( 'NONE', #10119, #7976, #22447 ) ;
#3275 = DIRECTION ( 'NONE',  ( -0.9730401042858024541, 0.2306359803922080898, 5.959266323858942451E-17 ) ) ;
#3276 = ORIENTED_EDGE ( 'NONE', *, *, #23444, .F. ) ;
#3277 = CARTESIAN_POINT ( 'NONE',  ( 34.17078830033462822, 8.269992485274588745, -8.820012287919192673 ) ) ;
#3278 = FACE_OUTER_BOUND ( 'NONE', #20136, .T. ) ;
#3279 = EDGE_LOOP ( 'NONE', ( #5422, #11798, #5153, #21974 ) ) ;
#3280 = PERSON_AND_ORGANIZATION_ROLE ( 'classification_officer' ) ;
#3281 = CARTESIAN_POINT ( 'NONE',  ( -69.90454993788326021, 6.134066389438223688, 0.7502499999999270308 ) ) ;
#3282 = ORIENTED_EDGE ( 'NONE', *, *, #3425, .T. ) ;
#3283 = ORIENTED_EDGE ( 'NONE', *, *, #529, .F. ) ;
#3284 = APPROVAL_STATUS ( 'not_yet_approved' ) ;
#3285 = PLANE ( 'NONE',  #22832 ) ;
#3286 = EDGE_CURVE ( 'NONE', #8780, #483, #11171, .T. ) ;
#3287 = EDGE_LOOP ( 'NONE', ( #3604, #18327 ) ) ;
#3288 = AXIS2_PLACEMENT_3D ( 'NONE', #9766, #4405, #11672 ) ;
#3289 = AXIS2_PLACEMENT_3D ( 'NONE', #7955, #4738, #15187 ) ;
#3290 = CARTESIAN_POINT ( 'NONE',  ( -20.00000000000000000, -20.00000000000000000, 5.000000000000000000 ) ) ;
#3291 = DATE_AND_TIME ( #22761, #21326 ) ;
#3292 = CC_DESIGN_PERSON_AND_ORGANIZATION_ASSIGNMENT ( #2622, #12131, ( #5001 ) ) ;
#3293 = PRODUCT_DEFINITION ( 'UNKNOWN', '', #8400, #8526 ) ;
#3294 = DATE_AND_TIME ( #6508, #11060 ) ;
#3295 = DIRECTION ( 'NONE',  ( -1.982541115402064913E-15, -6.814985084194598285E-15, 1.000000000000000000 ) ) ;
#3296 = ADVANCED_FACE ( 'NONE', ( #19930 ), #22043, .F. ) ;
#3297 = EDGE_CURVE ( 'NONE', #15392, #6625, #428, .T. ) ;
#3298 = CARTESIAN_POINT ( 'NONE',  ( 120.8143550994449953, 2.935590694028629599, 20.00000000000000000 ) ) ;
#3299 = EDGE_LOOP ( 'NONE', ( #20641, #18658 ) ) ;
#3300 = VECTOR ( 'NONE', #18970, 1000.000000000000227 ) ;
#3301 = VECTOR ( 'NONE', #19518, 1000.000000000000227 ) ;
#3302 = ORIENTED_EDGE ( 'NONE', *, *, #1254, .T. ) ;
#3303 = CARTESIAN_POINT ( 'NONE',  ( -23.50000000000000000, -20.00000000000000000, 0.000000000000000000 ) ) ;
#3304 = PLANE ( 'NONE',  #15819 ) ;
#3305 = VERTEX_POINT ( 'NONE', #16243 ) ;
#3306 = DIRECTION ( 'NONE',  ( -4.758660364968300250E-15, -2.033490192229560220E-14, 1.000000000000000000 ) ) ;
#3307 = DIRECTION ( 'NONE',  ( -0.005235963827102643048, 0.9999862922474495042, -7.723249237701186312E-15 ) ) ;
#3308 = AXIS2_PLACEMENT_3D ( 'NONE', #13116, #1935, #620 ) ;
#3309 = ORIENTED_EDGE ( 'NONE', *, *, #22532, .F. ) ;
#3310 = ORIENTED_EDGE ( 'NONE', *, *, #950, .T. ) ;
#3311 = PERSON_AND_ORGANIZATION ( #11966, #8758 ) ;
#3312 = EDGE_CURVE ( 'NONE', #10552, #5266, #4814, .T. ) ;
#3313 = ORIENTED_EDGE ( 'NONE', *, *, #1067, .T. ) ;
#3314 = VERTEX_POINT ( 'NONE', #7229 ) ;
#3315 = FACE_OUTER_BOUND ( 'NONE', #10843, .T. ) ;
#3316 = CIRCLE ( 'NONE', #16568, 2.009239999999998805 ) ;
#3317 = APPROVAL_STATUS ( 'not_yet_approved' ) ;
#3318 = B_SPLINE_CURVE_WITH_KNOTS ( 'NONE', 3,
 ( #19517, #10049, #12176, #1332, #19400, #3128, #6451, #20823, #14051, #15836, #3004, #19175, #6817, #21293, #2895, #15480, #8712, #10161, #5032, #13827, #23177, #17393, #23063, #12297, #1215, #1094, #8358, #3242, #15944, #12060 ),
 .UNSPECIFIED., .F., .F.,
 ( 4, 2, 2, 2, 2, 2, 2, 2, 2, 2, 2, 2, 2, 2, 4 ),
 ( 0.006516123109207543583, 0.006923489735540620284, 0.007330856361873697852, 0.007738222988206774552, 0.008145589614539851253, 0.008960322867206008124, 0.009367689493539088294, 0.009775056119872168464, 0.01018242274620524863, 0.01058978937253832880, 0.01140452262520448741, 0.01181188925153756064, 0.01221925587787063561, 0.01262662250420371057, 0.01303398913053678380 ),
 .UNSPECIFIED. ) ;
#3319 = CONICAL_SURFACE ( 'NONE', #1793, 1.154700538379250796, 1.047197551196598297 ) ;
#3320 = CARTESIAN_POINT ( 'NONE',  ( -67.17866478793438034, -8.351859544007679048, -6.061081896285953642E-15 ) ) ;
#3321 = DATE_AND_TIME ( #13575, #20465 ) ;
#3322 = AXIS2_PLACEMENT_3D ( 'NONE', #715, #15218, #6208 ) ;
#3323 = EDGE_CURVE ( 'NONE', #7064, #11903, #23374, .T. ) ;
#3324 = ADVANCED_FACE ( 'NONE', ( #9473 ), #9351, .F. ) ;
#3325 = FACE_OUTER_BOUND ( 'NONE', #4037, .T. ) ;
#3326 = CIRCLE ( 'NONE', #5225, 3.499999999999999556 ) ;
#3327 = PERSON_AND_ORGANIZATION ( #11966, #8758 ) ;
#3328 = VERTEX_POINT ( 'NONE', #16696 ) ;
#3329 = CIRCLE ( 'NONE', #18522, 3.000000000000001332 ) ;
#3330 = DIRECTION ( 'NONE',  ( -0.9730401042858024541, 0.2306359803922080898, 5.959266323858942451E-17 ) ) ;
#3331 = FACE_OUTER_BOUND ( 'NONE', #1230, .T. ) ;
#3332 = VERTEX_POINT ( 'NONE', #9010 ) ;
#3333 = AXIS2_PLACEMENT_3D ( 'NONE', #5989, #20601, #4443 ) ;
#3334 = LINE ( 'NONE', #14613, #2175 ) ;
#3335 = CARTESIAN_POINT ( 'NONE',  ( -19.49999999982379961, -0.1021026942259700004, -8.658030917271079259E-14 ) ) ;
#3336 = DIRECTION ( 'NONE',  ( 0.8846153846154060085, -0.4663213712685030377, 0.000000000000000000 ) ) ;
#3337 = ORIENTED_EDGE ( 'NONE', *, *, #14417, .F. ) ;
#3338 = ORIENTED_EDGE ( 'NONE', *, *, #17575, .T. ) ;
#3339 = CARTESIAN_POINT ( 'NONE',  ( -69.91240388362392366, 7.634045827809347706, 7.199999999999994849 ) ) ;
#3340 = CALENDAR_DATE ( 2026, 31, 10 ) ;
#3341 = ORIENTED_EDGE ( 'NONE', *, *, #15306, .T. ) ;
#3342 = ORIENTED_EDGE ( 'NONE', *, *, #9799, .T. ) ;
#3343 = CARTESIAN_POINT ( 'NONE',  ( -17.50058776013304396, 23.00629652915649004, -3.750000000000000000 ) ) ;
#3344 = DIRECTION ( 'NONE',  ( 0.000000000000000000, 0.000000000000000000, 1.000000000000000000 ) ) ;
#3345 = CARTESIAN_POINT ( 'NONE',  ( 114.1489752661110089, -25.18526831983100323, -3.400000000000049649 ) ) ;
#3346 = APPROVAL_ROLE ( '' ) ;
#3347 = CC_DESIGN_PERSON_AND_ORGANIZATION_ASSIGNMENT ( #15214, #8451, ( #2323 ) ) ;
#3348 = DIRECTION ( 'NONE',  ( -1.158391195604533947E-15, 6.607917932627710271E-32, 1.000000000000000000 ) ) ;
#3349 = DIRECTION ( 'NONE',  ( -0.9730401042858022320, 0.2306359803922080343, 5.959266323858941219E-17 ) ) ;
#3350 = CIRCLE ( 'NONE', #9429, 2.750000000000002220 ) ;
#3351 = CONICAL_SURFACE ( 'NONE', #12097, 2.624999999999998668, 0.4636476090008101458 ) ;
#3352 = DIRECTION ( 'NONE',  ( 1.000000000000000000, 0.000000000000000000, 0.000000000000000000 ) ) ;
#3353 = DIRECTION ( 'NONE',  ( 0.000000000000000000, 0.000000000000000000, -1.000000000000000000 ) ) ;
#3354 = APPROVAL_DATE_TIME ( #13475, #3641 ) ;
#3355 = DIRECTION ( 'NONE',  ( 0.2306359803922021778, 0.9730401042858037863, -1.407521210652540770E-17 ) ) ;
#3356 = DIRECTION ( 'NONE',  ( 0.000000000000000000, 0.000000000000000000, -1.000000000000000000 ) ) ;
#3357 = DIRECTION ( 'NONE',  ( -2.982858504577314686E-17, 2.441916418604790135E-15, 1.000000000000000000 ) ) ;
#3358 = EDGE_CURVE ( 'NONE', #23387, #17399, #14937, .T. ) ;
#3359 = FACE_OUTER_BOUND ( 'NONE', #10493, .T. ) ;
#3360 = CARTESIAN_POINT ( 'NONE',  ( 35.94015251278350576, 11.23436983788199761, -27.55602540378494325 ) ) ;
#3361 = ORIENTED_EDGE ( 'NONE', *, *, #15358, .F. ) ;
#3362 = DIRECTION ( 'NONE',  ( 0.8660135325225010172, 0.004534477687572227751, 0.5000000000000000000 ) ) ;
#3363 = CLOSED_SHELL ( 'NONE', ( #10547, #14906, #16759, #535, #19936, #7806, #206, #2474, #9481, #12393 ) ) ;
#3364 = EDGE_LOOP ( 'NONE', ( #18040, #9753 ) ) ;
#3365 = DIRECTION ( 'NONE',  ( 0.2306359803922033713, 0.9730401042858034533, -4.558064749665356219E-15 ) ) ;
#3366 = VECTOR ( 'NONE', #22037, 1000.000000000000000 ) ;
#3367 = DIRECTION ( 'NONE',  ( 3.210834492180725196E-17, -2.441916418604790135E-15, -1.000000000000000000 ) ) ;
#3368 = ORIENTED_EDGE ( 'NONE', *, *, #23171, .T. ) ;
#3369 = CARTESIAN_POINT ( 'NONE',  ( 113.2956221386590130, -28.78551670568849730, 2.700000000000000178 ) ) ;
#3370 = EDGE_LOOP ( 'NONE', ( #21626, #22225 ) ) ;
#3371 = CARTESIAN_POINT ( 'NONE',  ( -19.63010143622448211, 27.93838792505352941, -4.999999999995571542 ) ) ;
#3372 = DATE_AND_TIME ( #5158, #8493 ) ;
#3373 = AXIS2_PLACEMENT_3D ( 'NONE', #53, #7328, #18244 ) ;
#3374 = DIRECTION ( 'NONE',  ( 0.7806762821592939661, -0.6249356306644247017, -1.755540157688528527E-13 ) ) ;
#3375 = SHAPE_REPRESENTATION_RELATIONSHIP ( 'NONE' , 'NONE' ,  #12659, #4822 ) ;
#3376 = CARTESIAN_POINT ( 'NONE',  ( 43.66832999130209458, 21.22121844545429781, -13.00000000000000000 ) ) ;
#3377 = CARTESIAN_POINT ( 'NONE',  ( -20.00000000000000000, -20.00000000000000000, -2.500000000000000000 ) ) ;
#3378 = CYLINDRICAL_SURFACE ( 'NONE', #17986, 9.000000000000001776 ) ;
#3379 = EDGE_LOOP ( 'NONE', ( #16641, #2056, #22053, #23314 ) ) ;
#3380 = CARTESIAN_POINT ( 'NONE',  ( -25.44839750738890061, 25.46504853262640111, -2.500000000000059952 ) ) ;
#3381 = PERSON ( 'NAUO-PER26', 'UNSPECIFIED', 'UNSPECIFIED', ('UNSPECIFIED'), ('UNSPECIFIED'), ('UNSPECIFIED') ) ;
#3382 = CARTESIAN_POINT ( 'NONE',  ( 53.20239347634440463, 27.69690417850090114, 3.288194835581189691E-14 ) ) ;
#3383 = EDGE_CURVE ( 'NONE', #4635, #20542, #22723, .T. ) ;
#3384 = CYLINDRICAL_SURFACE ( 'NONE', #6487, 2.066999999999998394 ) ;
#3385 = ORIENTED_EDGE ( 'NONE', *, *, #2576, .T. ) ;
#3386 = CC_DESIGN_APPROVAL ( #17350, ( #22886 ) ) ;
#3387 = DIRECTION ( 'NONE',  ( -1.000000000000000000, 0.000000000000000000, -3.794988516547419626E-16 ) ) ;
#3388 = AXIS2_PLACEMENT_3D ( 'NONE', #10636, #19297, #10287 ) ;
#3389 = PLANE ( 'NONE',  #20937 ) ;
#3390 = CC_DESIGN_DATE_AND_TIME_ASSIGNMENT ( #1135, #22400, ( #18637 ) ) ;
#3391 = ORIENTED_EDGE ( 'NONE', *, *, #9186, .F. ) ;
#3392 = CARTESIAN_POINT ( 'NONE',  ( 28.74475271207850113, -0.4785145432217889905, 14.50000000000020073 ) ) ;
#3393 = VERTEX_POINT ( 'NONE', #16579 ) ;
#3394 = ORIENTED_EDGE ( 'NONE', *, *, #10947, .T. ) ;
#3395 = EDGE_CURVE ( 'NONE', #8919, #21873, #11057, .T. ) ;
#3396 = ADVANCED_FACE ( 'NONE', ( #7572, #9122 ), #16356, .T. ) ;
#3397 = APPROVAL_DATE_TIME ( #14217, #7357 ) ;
#3398 = DIRECTION ( 'NONE',  ( -0.9999862922474492821, -0.005235963827121951387, 1.466966272682004590E-16 ) ) ;
#3399 = ORIENTED_EDGE ( 'NONE', *, *, #15358, .T. ) ;
#3400 = CARTESIAN_POINT ( 'NONE',  ( -20.00000000000000000, -17.50000000000000000, -4.999999999995474731 ) ) ;
#3401 = PERSON_AND_ORGANIZATION ( #11966, #8758 ) ;
#3402 = PRODUCT ( '1602p_c_18', '1602p_c_18', '', ( #5974 ) ) ;
#3403 = CALENDAR_DATE ( 2026, 31, 10 ) ;
#3404 = VECTOR ( 'NONE', #4808, 1000.000000000000000 ) ;
#3405 = CARTESIAN_POINT ( 'NONE',  ( 2.664535259100379799E-14, -1.554450629062440126E-15, 2.500000000000000000 ) ) ;
#3406 = AXIS2_PLACEMENT_3D ( 'NONE', #937, #12246, #2853 ) ;
#3407 = DIRECTION ( 'NONE',  ( 1.187319687680494078E-16, 2.805478249478275539E-20, 1.000000000000000000 ) ) ;
#3408 = ORIENTED_EDGE ( 'NONE', *, *, #9230, .F. ) ;
#3409 = LINE ( 'NONE', #4880, #23448 ) ;
#3410 = EDGE_CURVE ( 'NONE', #20573, #1580, #14810, .T. ) ;
#3411 = EDGE_LOOP ( 'NONE', ( #20484, #342, #9659, #6734 ) ) ;
#3412 = DIRECTION ( 'NONE',  ( 0.9730401042858035643, -0.2306359803922028717, -5.432877459303547053E-17 ) ) ;
#3413 = DIRECTION ( 'NONE',  ( -0.9997651245880698756, -0.02167246311338769799, 2.310076446361489313E-17 ) ) ;
#3414 = ORIENTED_EDGE ( 'NONE', *, *, #21285, .T. ) ;
#3415 = CC_DESIGN_DATE_AND_TIME_ASSIGNMENT ( #410, #2456, ( #10854 ) ) ;
#3416 = CC_DESIGN_APPROVAL ( #7944, ( #1978 ) ) ;
#3417 = CC_DESIGN_PERSON_AND_ORGANIZATION_ASSIGNMENT ( #4076, #1844, ( #19398 ) ) ;
#3418 = CARTESIAN_POINT ( 'NONE',  ( -21.99941281109913760, -0.1562838609880492502, 2.500000000000000000 ) ) ;
#3419 = LINE ( 'NONE', #14469, #6961 ) ;
#3420 = ORIENTED_EDGE ( 'NONE', *, *, #18127, .T. ) ;
#3421 = AXIS2_PLACEMENT_3D ( 'NONE', #18226, #1947, #10649 ) ;
#3422 = VERTEX_POINT ( 'NONE', #5793 ) ;
#3423 = ADVANCED_FACE ( 'NONE', ( #14585 ), #3072, .F. ) ;
#3424 = AXIS2_PLACEMENT_3D ( 'NONE', #14001, #22550, #6294 ) ;
#3425 = EDGE_CURVE ( 'NONE', #9613, #21153, #3761, .T. ) ;
#3426 = APPROVAL_STATUS ( 'not_yet_approved' ) ;
#3427 = ORIENTED_EDGE ( 'NONE', *, *, #10719, .T. ) ;
#3428 = ORIENTED_EDGE ( 'NONE', *, *, #4168, .T. ) ;
#3429 = PRODUCT_RELATED_PRODUCT_CATEGORY ( 'detail', '', ( #3606 ) ) ;
#3430 = CARTESIAN_POINT ( 'NONE',  ( 6.500000000000000000, -17.30000000000000071, -5.000000000000000000 ) ) ;
#3431 = APPROVAL_ROLE ( '' ) ;
#3432 = DIRECTION ( 'NONE',  ( 0.000000000000000000, -6.936119456124777094E-16, 1.000000000000000000 ) ) ;
#3433 = APPROVAL_DATE_TIME ( #22349, #6447 ) ;
#3434 = AXIS2_PLACEMENT_3D ( 'NONE', #2259, #2, #14738 ) ;
#3435 = LOCAL_TIME ( 14, 11, 27.00000000000000000, #18068 ) ;
#3436 = SHAPE_REPRESENTATION_RELATIONSHIP ( 'NONE' , 'NONE' ,  #20540, #14745 ) ;
#3437 = APPROVAL_PERSON_ORGANIZATION ( #2831, #16471, #15526 ) ;
#3438 = CARTESIAN_POINT ( 'NONE',  ( -20.00000000000000000, -20.00000000000000000, 2.500000000000000000 ) ) ;
#3439 = CIRCLE ( 'NONE', #826, 4.999999999999997335 ) ;
#3440 = DATE_AND_TIME ( #6787, #18612 ) ;
#3441 = EDGE_CURVE ( 'NONE', #17345, #11267, #6881, .T. ) ;
#3442 = ORIENTED_EDGE ( 'NONE', *, *, #22183, .F. ) ;
#3443 = DIRECTION ( 'NONE',  ( -1.000000000000000000, 0.000000000000000000, 0.000000000000000000 ) ) ;
#3444 = FACE_BOUND ( 'NONE', #9533, .T. ) ;
#3445 = TOROIDAL_SURFACE ( 'NONE', #1910, 2.600000000000000089, 0.1000000000000000056 ) ;
#3446 = EDGE_LOOP ( 'NONE', ( #3885, #22914, #20549, #15372 ) ) ;
#3447 = ADVANCED_FACE ( 'NONE', ( #11390 ), #15155, .T. ) ;
#3448 = DIRECTION ( 'NONE',  ( -0.9730401042858035643, 0.2306359803922028717, 5.959266323858677443E-17 ) ) ;
#3449 = CYLINDRICAL_SURFACE ( 'NONE', #17209, 6.499999999999997335 ) ;
#3450 = CARTESIAN_POINT ( 'NONE',  ( -62.99678855639989905, 23.76850991288289805, 6.352789585277969841E-15 ) ) ;
#3451 = ORIENTED_EDGE ( 'NONE', *, *, #6935, .F. ) ;
#3452 = ORIENTED_EDGE ( 'NONE', *, *, #6794, .F. ) ;
#3453 = DIRECTION ( 'NONE',  ( 0.9730401042858035643, -0.2306359803922028717, -5.958148513035547083E-17 ) ) ;
#3454 = ORIENTED_EDGE ( 'NONE', *, *, #1795, .F. ) ;
#3455 = EDGE_CURVE ( 'NONE', #20882, #6499, #22406, .T. ) ;
#3456 = MECHANICAL_CONTEXT ( 'NONE', #156, 'mechanical' ) ;
#3457 = LOCAL_TIME ( 14, 11, 27.00000000000000000, #2348 ) ;
#3459 = ADVANCED_FACE ( 'NONE', ( #6378, #7811 ), #4366, .F. ) ;
#3458 = ORIENTED_EDGE ( 'NONE', *, *, #11403, .T. ) ;
#3460 = ORIENTED_EDGE ( 'NONE', *, *, #23001, .F. ) ;
#3461 = CARTESIAN_POINT ( 'NONE',  ( 52.49909637502329929, -7.592283011512489743, 13.00000000000019895 ) ) ;
#3462 = DIRECTION ( 'NONE',  ( 0.000000000000000000, 1.000000000000000000, 0.000000000000000000 ) ) ;
#3463 = PRODUCT_DEFINITION_FORMATION_WITH_SPECIFIED_SOURCE ( 'ANY', '', #10241, .NOT_KNOWN. ) ;
#3464 = CYLINDRICAL_SURFACE ( 'NONE', #22045, 2.066999999999999726 ) ;
#3465 = DATE_AND_TIME ( #23053, #1956 ) ;
#3466 = DIRECTION ( 'NONE',  ( 1.000000000000000000, 0.000000000000000000, 0.000000000000000000 ) ) ;
#3467 = APPROVAL_PERSON_ORGANIZATION ( #5180, #23109, #23453 ) ;
#3468 = DIRECTION ( 'NONE',  ( -0.4865200521429013936, 0.1153179901961013387, -0.8660254037844388186 ) ) ;
#3469 = ORIENTED_EDGE ( 'NONE', *, *, #12340, .F. ) ;
#3470 = DIRECTION ( 'NONE',  ( 0.000000000000000000, 0.000000000000000000, 1.000000000000000000 ) ) ;
#3471 = LINE ( 'NONE', #19744, #2597 ) ;
#3472 = APPLICATION_PROTOCOL_DEFINITION ( 'international standard', 'config_control_design', 1994, #11119 ) ;
#3473 = LOCAL_TIME ( 14, 11, 27.00000000000000000, #1610 ) ;
#3474 = LINE ( 'NONE', #11090, #2670 ) ;
#3475 = VECTOR ( 'NONE', #1630, 1000.000000000000000 ) ;
#3476 = DIRECTION ( 'NONE',  ( 0.000000000000000000, 1.734723475976806848E-16, 1.000000000000000000 ) ) ;
#3477 = VECTOR ( 'NONE', #7159, 1000.000000000000000 ) ;
#3478 = CARTESIAN_POINT ( 'NONE',  ( 38.03772126950729415, -1.595291315507239682, 13.00000000000000000 ) ) ;
#3479 = DIRECTION ( 'NONE',  ( 0.9730401042858036753, -0.2306359803922031493, 2.804983810440361760E-16 ) ) ;
#3480 = CARTESIAN_POINT ( 'NONE',  ( 36.15732495067950225, 25.37491064193179824, -13.00000000000049916 ) ) ;
#3481 = EDGE_LOOP ( 'NONE', ( #9777, #10910, #16130, #13421 ) ) ;
#3482 = ORGANIZATION ( 'NAUO-ORG26', 'UNSPECIFIED', 'UNSPECIFIED' ) ;
#3483 = DIRECTION ( 'NONE',  ( -0.9730401042858024541, 0.2306359803922080898, 5.959266323858932590E-17 ) ) ;
#3484 = UNCERTAINTY_MEASURE_WITH_UNIT (LENGTH_MEASURE( 1.000000000000000082E-05 ), #6065, 'distance_accuracy_value', 'NONE');
#3485 = EDGE_CURVE ( 'NONE', #21440, #13431, #5728, .T. ) ;
#3486 = ORIENTED_EDGE ( 'NONE', *, *, #20683, .T. ) ;
#3487 = DIRECTION ( 'NONE',  ( -1.000000000000000000, -9.248903203239929993E-11, 2.269747459791049881E-13 ) ) ;
#3488 = DIRECTION ( 'NONE',  ( -0.6862566701892794940, -0.7273594590164634832, 3.657607522630173034E-15 ) ) ;
#3489 = ORIENTED_EDGE ( 'NONE', *, *, #11916, .F. ) ;
#3490 = CARTESIAN_POINT ( 'NONE',  ( 115.8700071457750056, -9.252658700902388844, 3.427049305831379237E-14 ) ) ;
#3491 = ORIENTED_EDGE ( 'NONE', *, *, #1275, .T. ) ;
#3492 = PRODUCT_DEFINITION_FORMATION_WITH_SPECIFIED_SOURCE ( 'ANY', '', #19920, .NOT_KNOWN. ) ;
#3493 = DIRECTION ( 'NONE',  ( -0.9730401042858036753, 0.2306359803922028995, 5.958148513035547083E-17 ) ) ;
#3494 = PERSON_AND_ORGANIZATION ( #11966, #8758 ) ;
#3495 = AXIS2_PLACEMENT_3D ( 'NONE', #10628, #14399, #5501 ) ;
#3496 = CARTESIAN_POINT ( 'NONE',  ( 33.27836309399498305, 10.32372331478670979, -29.25000000000050449 ) ) ;
#3497 = VECTOR ( 'NONE', #21930, 1000.000000000000000 ) ;
#3498 = EDGE_CURVE ( 'NONE', #16156, #12721, #19020, .T. ) ;
#3499 = AXIS2_PLACEMENT_3D ( 'NONE', #3461, #10732, #1673 ) ;
#3500 = AXIS2_PLACEMENT_3D ( 'NONE', #3042, #1481, #4716 ) ;
#3501 =( LENGTH_UNIT ( ) NAMED_UNIT ( * ) SI_UNIT ( .MILLI., .METRE. ) );
#3502 = ORIENTED_EDGE ( 'NONE', *, *, #20721, .T. ) ;
#3503 = CARTESIAN_POINT ( 'NONE',  ( 5.000000000000000000, -31.09999999999999787, -21.50000000000000000 ) ) ;
#3504 = AXIS2_PLACEMENT_3D ( 'NONE', #13104, #720, #14987 ) ;
#3505 = CARTESIAN_POINT ( 'NONE',  ( 55.93909781928478253, -6.283383317918767474, -13.00000000000000000 ) ) ;
#3506 = PERSON_AND_ORGANIZATION ( #11966, #8758 ) ;
#3507 = CARTESIAN_POINT ( 'NONE',  ( -0.03403376487617940094, 6.499910899608420500, -8.889172688581379631E-14 ) ) ;
#3508 = DIRECTION ( 'NONE',  ( 1.751019220569994795E-16, 2.300154215587015208E-15, 1.000000000000000000 ) ) ;
#3509 = DIRECTION ( 'NONE',  ( -0.2306359803922066187, -0.9730401042858026761, 0.000000000000000000 ) ) ;
#3510 = CC_DESIGN_APPROVAL ( #14898, ( #1997 ) ) ;
#3511 = LINE ( 'NONE', #16442, #11445 ) ;
#3512 = ORIENTED_EDGE ( 'NONE', *, *, #1657, .T. ) ;
#3513 = FACE_BOUND ( 'NONE', #10665, .T. ) ;
#3514 = AXIS2_PLACEMENT_3D ( 'NONE', #1542, #8811, #14617 ) ;
#3515 = CARTESIAN_POINT ( 'NONE',  ( -31.64684134471649912, 7.334398819369050138, -5.000000000000000000 ) ) ;
#3516 = AXIS2_PLACEMENT_3D ( 'NONE', #2667, #17160, #19069 ) ;
#3517 = VERTEX_POINT ( 'NONE', #4122 ) ;
#3518 = VECTOR ( 'NONE', #2084, 1000.000000000000000 ) ;
#3519 = CARTESIAN_POINT ( 'NONE',  ( -69.82862846239015653, -8.365734848149525504, -7.200000000000000178 ) ) ;
#3520 = EDGE_LOOP ( 'NONE', ( #6079, #3203, #4402, #1577, #1514 ) ) ;
#3521 = APPROVAL_STATUS ( 'not_yet_approved' ) ;
#3522 = CIRCLE ( 'NONE', #13766, 2.066999999999998838 ) ;
#3523 = CARTESIAN_POINT ( 'NONE',  ( 30.84445860938240003, -2.459566909556700320, -13.00000000000039968 ) ) ;
#3524 = VERTEX_POINT ( 'NONE', #19098 ) ;
#3525 = SPHERICAL_SURFACE ( 'NONE', #13960, 15.25000000000000000 ) ;
#3526 = AXIS2_PLACEMENT_3D ( 'NONE', #3265, #17414, #6729 ) ;
#3527 = CALENDAR_DATE ( 2026, 31, 10 ) ;
#3528 = EDGE_CURVE ( 'NONE', #12983, #7920, #13621, .T. ) ;
#3529 = AXIS2_PLACEMENT_3D ( 'NONE', #19488, #1654, #21137 ) ;
#3530 = EDGE_CURVE ( 'NONE', #14820, #22403, #13268, .T. ) ;
#3531 = LOCAL_TIME ( 14, 11, 27.00000000000000000, #13140 ) ;
#3532 = DATE_AND_TIME ( #9000, #17879 ) ;
#3533 = DIRECTION ( 'NONE',  ( -1.000000000000000000, 2.270069654138870255E-15, 0.000000000000000000 ) ) ;
#3534 = CIRCLE ( 'NONE', #10368, 1.000000000000000000 ) ;
#3535 = AXIS2_PLACEMENT_3D ( 'NONE', #19886, #21525, #3716 ) ;
#3536 = CIRCLE ( 'NONE', #19094, 2.500000000000001776 ) ;
#3537 = DIRECTION ( 'NONE',  ( -0.2306359803922080343, -0.9730401042858022320, -5.907067092757111157E-15 ) ) ;
#3538 = ORIENTED_EDGE ( 'NONE', *, *, #12897, .T. ) ;
#3539 = FACE_OUTER_BOUND ( 'NONE', #17262, .T. ) ;
#3540 = ADVANCED_FACE ( 'NONE', ( #18758 ), #2583, .F. ) ;
#3541 = EDGE_CURVE ( 'NONE', #6526, #8301, #12203, .T. ) ;
#3542 = ORIENTED_EDGE ( 'NONE', *, *, #22589, .T. ) ;
#3543 = AXIS2_PLACEMENT_3D ( 'NONE', #21318, #1002, #10187 ) ;
#3544 = CYLINDRICAL_SURFACE ( 'NONE', #1378, 4.250000000000000000 ) ;
#3545 = CARTESIAN_POINT ( 'NONE',  ( -19.49999999982360066, -0.1021026942259700004, -2.500000000000000000 ) ) ;
#3546 = DIRECTION ( 'NONE',  ( -0.9997651245102238127, -0.02167246670447303680, 0.000000000000000000 ) ) ;
#3547 = ORIENTED_EDGE ( 'NONE', *, *, #13917, .T. ) ;
#3548 = PERSON_AND_ORGANIZATION_ROLE ( 'creator' ) ;
#3549 = AXIS2_PLACEMENT_3D ( 'NONE', #3878, #1738, #9003 ) ;
#3550 = DIRECTION ( 'NONE',  ( 0.000000000000000000, 0.000000000000000000, -1.000000000000000000 ) ) ;
#3551 = LINE ( 'NONE', #14119, #3553 ) ;
#3552 =( REPRESENTATION_RELATIONSHIP ('NONE','NONE', #19303, #9451 ) REPRESENTATION_RELATIONSHIP_WITH_TRANSFORMATION ( #15141 )SHAPE_REPRESENTATION_RELATIONSHIP( ) );
#3553 = VECTOR ( 'NONE', #10813, 1000.000000000000114 ) ;
#3554 = ORIENTED_EDGE ( 'NONE', *, *, #14245, .T. ) ;
#3555 = CALENDAR_DATE ( 2026, 31, 10 ) ;
#3556 = VERTEX_POINT ( 'NONE', #22627 ) ;
#3557 = CIRCLE ( 'NONE', #7365, 5.000000000000001776 ) ;
#3558 = ORIENTED_EDGE ( 'NONE', *, *, #3993, .F. ) ;
#3559 = CARTESIAN_POINT ( 'NONE',  ( 33.37436288052550282, -3.059220458576419777, -13.00000000000039968 ) ) ;
#3560 = APPROVAL_ROLE ( '' ) ;
#3561 = ADVANCED_FACE ( 'NONE', ( #2467 ), #2820, .F. ) ;
#3562 = CARTESIAN_POINT ( 'NONE',  ( 96.33985310849000427, -20.10796027570521716, 13.00000000000000000 ) ) ;
#3563 = SECURITY_CLASSIFICATION_LEVEL ( 'unclassified' ) ;
#3564 = FACE_OUTER_BOUND ( 'NONE', #15188, .T. ) ;
#3565 = CC_DESIGN_PERSON_AND_ORGANIZATION_ASSIGNMENT ( #12533, #16200, ( #6956 ) ) ;
#3566 = APPROVAL ( #12285, 'UNSPECIFIED' ) ;
#3567 =( NAMED_UNIT ( * ) PLANE_ANGLE_UNIT ( ) SI_UNIT ( $, .RADIAN. ) );
#3568 = CYLINDRICAL_SURFACE ( 'NONE', #2393, 2.750000000000000000 ) ;
#3569 = VECTOR ( 'NONE', #7839, 1000.000000000000227 ) ;
#3570 = ADVANCED_FACE ( 'NONE', ( #667 ), #18971, .F. ) ;
#3571 = EDGE_CURVE ( 'NONE', #12545, #6522, #9959, .T. ) ;
#3572 = PERSON_AND_ORGANIZATION_ROLE ( 'classification_officer' ) ;
#3573 = VERTEX_POINT ( 'NONE', #20635 ) ;
#3574 = CARTESIAN_POINT ( 'NONE',  ( -20.00000000000000000, -20.00000000000000000, 0.000000000000000000 ) ) ;
#3575 = DIRECTION ( 'NONE',  ( 2.269700743865589996E-13, 2.220446049247695246E-15, 1.000000000000000000 ) ) ;
#3576 = ORIENTED_EDGE ( 'NONE', *, *, #10562, .F. ) ;
#3577 = CARTESIAN_POINT ( 'NONE',  ( 96.81657767996070163, -18.09668638014640152, -13.00000000000000000 ) ) ;
#3578 = PLANE ( 'NONE',  #12307 ) ;
#3579 = FACE_OUTER_BOUND ( 'NONE', #5128, .T. ) ;
#3580 = EDGE_LOOP ( 'NONE', ( #2935, #10284 ) ) ;
#3581 = ORIENTED_EDGE ( 'NONE', *, *, #16600, .T. ) ;
#3582 = DIRECTION ( 'NONE',  ( 0.000000000000000000, -2.739767185169287006E-14, -1.000000000000000000 ) ) ;
#3583 = ORIENTED_EDGE ( 'NONE', *, *, #19736, .T. ) ;
#3584 = PERSON_AND_ORGANIZATION_ROLE ( 'creator' ) ;
#3585 = EDGE_LOOP ( 'NONE', ( #7907, #8312, #20226, #6658 ) ) ;
#3586 = VERTEX_POINT ( 'NONE', #18862 ) ;
#3587 = CARTESIAN_POINT ( 'NONE',  ( 36.79228697538940196, -6.849707878650520776, 3.000000000000000000 ) ) ;
#3588 = DIRECTION ( 'NONE',  ( -0.9730401042858036753, 0.2306359803922028995, 5.959266323858677443E-17 ) ) ;
#3589 = CARTESIAN_POINT ( 'NONE',  ( -27.00000000000000000, -28.60000000000000142, -6.250000000000000000 ) ) ;
#3590 = CALENDAR_DATE ( 2026, 31, 10 ) ;
#3591 = LINE ( 'NONE', #14512, #21856 ) ;
#3592 = EDGE_CURVE ( 'NONE', #13456, #12123, #1011, .T. ) ;
#3593 = DIRECTION ( 'NONE',  ( 0.9999862922474493931, 0.005235963827108502076, 0.000000000000000000 ) ) ;
#3594 = EDGE_CURVE ( 'NONE', #19697, #2044, #17057, .T. ) ;
#3595 = EDGE_CURVE ( 'NONE', #6087, #10804, #1160, .T. ) ;
#3596 = CARTESIAN_POINT ( 'NONE',  ( 44.19498725252769589, 23.44315552359092791, -13.00000000000000000 ) ) ;
#3597 = PERSON_AND_ORGANIZATION ( #11966, #8758 ) ;
#3598 = DIRECTION ( 'NONE',  ( -0.2306359803922031215, -0.9730401042858035643, -4.620383928407073520E-16 ) ) ;
#3599 = CARTESIAN_POINT ( 'NONE',  ( 35.59419854219520118, 9.774809681453469068, 10.74538000000019977 ) ) ;
#3600 = AXIS2_PLACEMENT_3D ( 'NONE', #18551, #471, #21616 ) ;
#3601 = DIRECTION ( 'NONE',  ( -0.9999863470141812094, -0.005225493778937320352, -1.706795874242040883E-17 ) ) ;
#3602 = CARTESIAN_POINT ( 'NONE',  ( -67.26895854462254931, 12.68829727884599201, -2.499999999999999556 ) ) ;
#3603 = CARTESIAN_POINT ( 'NONE',  ( 36.78282996199610722, 11.03463321983590006, 28.46999999999999886 ) ) ;
#3604 = ORIENTED_EDGE ( 'NONE', *, *, #23415, .T. ) ;
#3605 = CARTESIAN_POINT ( 'NONE',  ( 34.39395800938287096, 11.46298095551878227, 8.896276805998372339 ) ) ;
#3606 = PRODUCT ( 'Pin', 'Pin', '', ( #17260 ) ) ;
#3607 = ORIENTED_EDGE ( 'NONE', *, *, #2070, .T. ) ;
#3608 = DIRECTION ( 'NONE',  ( -0.1153179901961009640, -0.4865200521429018377, -0.8660254037844385966 ) ) ;
#3609 = CARTESIAN_POINT ( 'NONE',  ( 11.50000000000000000, -23.36217782649110219, -2.500000000000000000 ) ) ;
#3610 = ORIENTED_EDGE ( 'NONE', *, *, #11121, .T. ) ;
#3612 = ORIENTED_EDGE ( 'NONE', *, *, #4711, .T. ) ;
#3611 = EDGE_CURVE ( 'NONE', #747, #11532, #553, .T. ) ;
#3613 = CIRCLE ( 'NONE', #8563, 2.501000000000000334 ) ;
#3614 = CARTESIAN_POINT ( 'NONE',  ( 36.68971944905818816, 14.39675017681111058, 27.87499999999997513 ) ) ;
#3615 = APPROVAL_ROLE ( '' ) ;
#3616 = CARTESIAN_POINT ( 'NONE',  ( 38.67394081127457639, 19.73298157975121470, 13.00000000000000000 ) ) ;
#3617 = EDGE_CURVE ( 'NONE', #16606, #18892, #9964, .T. ) ;
#3618 = DIRECTION ( 'NONE',  ( 0.9730401042858036753, -0.2306359803922031493, -5.959266323858673745E-17 ) ) ;
#3619 = ADVANCED_FACE ( 'NONE', ( #3278 ), #8386, .F. ) ;
#3620 = CARTESIAN_POINT ( 'NONE',  ( 118.5310588935630136, -6.697506338400810222, 19.59999999999999787 ) ) ;
#3621 = CALENDAR_DATE ( 2026, 31, 10 ) ;
#3622 = EDGE_CURVE ( 'NONE', #18417, #16923, #23201, .T. ) ;
#3623 = DIRECTION ( 'NONE',  ( -1.187319687680499994E-16, -2.805478249478640262E-20, -1.000000000000000000 ) ) ;
#3624 = CARTESIAN_POINT ( 'NONE',  ( 29.09552749756809931, -4.418411798633290033, -13.00000000000039968 ) ) ;
#3625 = DIRECTION ( 'NONE',  ( 0.9730401042858035643, -0.2306359803922028717, -5.432877459303547053E-17 ) ) ;
#3626 = DIRECTION ( 'NONE',  ( 3.211814849206744928E-17, -2.442368445299930211E-15, -1.000000000000000000 ) ) ;
#3627 = ORIENTED_EDGE ( 'NONE', *, *, #18200, .F. ) ;
#3628 = DIRECTION ( 'NONE',  ( 2.269747459788990007E-13, 2.220446049250330436E-15, 1.000000000000000000 ) ) ;
#3629 = LINE ( 'NONE', #1722, #21316 ) ;
#3630 = ORIENTED_EDGE ( 'NONE', *, *, #6357, .T. ) ;
#3631 = AXIS2_PLACEMENT_3D ( 'NONE', #14557, #18118, #5633 ) ;
#3632 = VERTEX_POINT ( 'NONE', #8745 ) ;
#3633 = CARTESIAN_POINT ( 'NONE',  ( -58.40809801011923241, -21.80622160268157828, -5.536374493610581309E-15 ) ) ;
#3634 = CARTESIAN_POINT ( 'NONE',  ( 36.78282996199610722, 11.03463321983559986, -28.47000000000049980 ) ) ;
#3635 = VERTEX_POINT ( 'NONE', #12335 ) ;
#3636 = PERSON_AND_ORGANIZATION ( #11966, #8758 ) ;
#3637 = FACE_OUTER_BOUND ( 'NONE', #13224, .T. ) ;
#3638 = VERTEX_POINT ( 'NONE', #12214 ) ;
#3639 = DIRECTION ( 'NONE',  ( -1.000000000000000000, -9.259433497721235207E-11, 1.142026288351377283E-14 ) ) ;
#3640 = APPROVAL_DATE_TIME ( #21914, #5163 ) ;
#3641 = APPROVAL ( #4790, 'UNSPECIFIED' ) ;
#3642 =( GEOMETRIC_REPRESENTATION_CONTEXT ( 3 ) GLOBAL_UNCERTAINTY_ASSIGNED_CONTEXT ( ( #17195 ) ) GLOBAL_UNIT_ASSIGNED_CONTEXT ( ( #14656, #4084, #20245 ) ) REPRESENTATION_CONTEXT ( 'NONE', 'WORKASPACE' ) );
#3643 = APPROVAL_STATUS ( 'not_yet_approved' ) ;
#3644 = CYLINDRICAL_SURFACE ( 'NONE', #8177, 1.000000000000000888 ) ;
#3645 = AXIS2_PLACEMENT_3D ( 'NONE', #596, #6304, #15329 ) ;
#3646 = DIRECTION ( 'NONE',  ( 0.000000000000000000, 0.000000000000000000, -1.000000000000000000 ) ) ;
#3647 = VERTEX_POINT ( 'NONE', #17886 ) ;
#3648 = FACE_OUTER_BOUND ( 'NONE', #2859, .T. ) ;
#3649 = ORIENTED_EDGE ( 'NONE', *, *, #3592, .F. ) ;
#3650 = CARTESIAN_POINT ( 'NONE',  ( -14.10663218835320087, 21.82654748245090204, -5.000000000000060396 ) ) ;
#3651 = CARTESIAN_POINT ( 'NONE',  ( 117.0319250210129951, -13.02226701625859917, 18.89999999999999858 ) ) ;
#3652 = DIRECTION ( 'NONE',  ( 2.982858504489139758E-17, -2.441916418604790135E-15, -1.000000000000000000 ) ) ;
#3653 = ORIENTED_EDGE ( 'NONE', *, *, #11974, .T. ) ;
#3654 = ADVANCED_FACE ( 'NONE', ( #8880, #2930, #6853 ), #19435, .T. ) ;
#3655 = AXIS2_PLACEMENT_3D ( 'NONE', #6189, #474, #7736 ) ;
#3656 = AXIS2_PLACEMENT_3D ( 'NONE', #21414, #5375, #1691 ) ;
#3657 = CARTESIAN_POINT ( 'NONE',  ( 30.31182762792540331, -4.706706774123410320, 13.00000000000019895 ) ) ;
#3658 = EDGE_LOOP ( 'NONE', ( #22201, #7290, #1293, #703 ) ) ;
#3659 = PERSON_AND_ORGANIZATION ( #11966, #8758 ) ;
#3660 = ORIENTED_EDGE ( 'NONE', *, *, #8984, .T. ) ;
#3661 = EDGE_LOOP ( 'NONE', ( #11902, #21846, #23394, #7749, #10464 ) ) ;
#3662 = LINE ( 'NONE', #5110, #7697 ) ;
#3663 = CALENDAR_DATE ( 2026, 31, 10 ) ;
#3664 = FACE_BOUND ( 'NONE', #1812, .T. ) ;
#3665 = CONTEXT_DEPENDENT_SHAPE_REPRESENTATION ( #12069, #4186 ) ;
#3666 = CARTESIAN_POINT ( 'NONE',  ( 33.37436288052550282, -3.059220458576299873, 13.00000000000019895 ) ) ;
#3667 = AXIS2_PLACEMENT_3D ( 'NONE', #15140, #20270, #16564 ) ;
#3668 = AXIS2_PLACEMENT_3D ( 'NONE', #17797, #3413, #1395 ) ;
#3669 = AXIS2_PLACEMENT_3D ( 'NONE', #13327, #5958, #13100 ) ;
#3670 = LINE ( 'NONE', #1880, #5426 ) ;
#3671 = PERSON_AND_ORGANIZATION_ROLE ( 'creator' ) ;
#3672 = ORIENTED_EDGE ( 'NONE', *, *, #21381, .T. ) ;
#3673 = DIRECTION ( 'NONE',  ( -6.662111519016958720E-09, 1.000000000000000000, -2.523234146875356491E-15 ) ) ;
#3674 = VERTEX_POINT ( 'NONE', #14086 ) ;
#3675 = ADVANCED_BREP_SHAPE_REPRESENTATION ( '', ( #9134, #12739 ), #6306 ) ;
#3676 = EDGE_CURVE ( 'NONE', #2375, #20234, #21688, .T. ) ;
#3677 = CARTESIAN_POINT ( 'NONE',  ( -20.00000000000000000, -20.00000000000000000, 2.500000000000000000 ) ) ;
#3678 = FACE_OUTER_BOUND ( 'NONE', #20537, .T. ) ;
#3679 =( BOUNDED_CURVE ( )  B_SPLINE_CURVE ( 2, ( #14616, #9273, #14961 ),
 .UNSPECIFIED., .F., .F. ) 
 B_SPLINE_CURVE_WITH_KNOTS ( ( 3, 3 ),
 ( 0.000000000000000000, 0.1168436138077860315 ),
 .UNSPECIFIED. ) 
 CURVE ( )  GEOMETRIC_REPRESENTATION_ITEM ( )  RATIONAL_B_SPLINE_CURVE ( ( 1.000000000000000000, 1.077350269189620402, 1.077350269189624843 ) ) 
 REPRESENTATION_ITEM ( '' )  );
#3680 = DIRECTION ( 'NONE',  ( -1.187319687680494078E-16, -2.805478249478345354E-20, -1.000000000000000000 ) ) ;
#3681 = VERTEX_POINT ( 'NONE', #8633 ) ;
#3682 = ORIENTED_EDGE ( 'NONE', *, *, #20388, .T. ) ;
#3683 = DIRECTION ( 'NONE',  ( -0.2306359803922031770, -0.9730401042858034533, 0.000000000000000000 ) ) ;
#3684 = VERTEX_POINT ( 'NONE', #17666 ) ;
#3685 = APPROVAL ( #13958, 'UNKNOWN' ) ;
#3686 = DATE_TIME_ROLE ( 'classification_date' ) ;
#3687 = AXIS2_PLACEMENT_3D ( 'NONE', #13492, #20727, #5393 ) ;
#3688 = ORIENTED_EDGE ( 'NONE', *, *, #8699, .F. ) ;
#3689 = ORIENTED_EDGE ( 'NONE', *, *, #19139, .T. ) ;
#3690 = DIRECTION ( 'NONE',  ( -0.9997651245880592175, -0.02167246311387461752, 0.000000000000000000 ) ) ;
#3691 = AXIS2_PLACEMENT_3D ( 'NONE', #12605, #16038, #19601 ) ;
#3692 = CARTESIAN_POINT ( 'NONE',  ( 31.49315201223960159, -2.613324229818170252, -11.84529946162114911 ) ) ;
#3693 = PERSON_AND_ORGANIZATION ( #11966, #8758 ) ;
#3694 = ADVANCED_FACE ( 'NONE', ( #17423 ), #1367, .F. ) ;
#3695 = DIRECTION ( 'NONE',  ( -0.2306359803922033158, -0.9730401042858034533, 0.000000000000000000 ) ) ;
#3696 = EDGE_CURVE ( 'NONE', #15392, #18750, #16707, .T. ) ;
#3697 = DIRECTION ( 'NONE',  ( -0.9730401042858023430, 0.2306359803922080620, 5.959266323858944916E-17 ) ) ;
#3698 = VECTOR ( 'NONE', #9036, 1000.000000000000227 ) ;
#3699 = ORIENTED_EDGE ( 'NONE', *, *, #3528, .T. ) ;
#3701 = DIRECTION ( 'NONE',  ( -0.5249589903860224505, 0.8511275218278915311, 1.187479569643817911E-16 ) ) ;
#3700 = CIRCLE ( 'NONE', #16981, 2.500000000000000000 ) ;
#3702 = PERSON_AND_ORGANIZATION_ROLE ( 'creator' ) ;
#3703 = AXIS2_PLACEMENT_3D ( 'NONE', #5629, #21782, #9079 ) ;
#3704 = DIRECTION ( 'NONE',  ( 0.000000000000000000, 0.000000000000000000, -1.000000000000000000 ) ) ;
#3705 = CARTESIAN_POINT ( 'NONE',  ( -11.00000000000000000, -27.34999999999999787, 6.250000000000000000 ) ) ;
#3706 = DIRECTION ( 'NONE',  ( -0.005235963827108352890, 0.9999862922474493931, 5.936218956694023463E-19 ) ) ;
#3707 = ADVANCED_FACE ( 'NONE', ( #16105 ), #3389, .T. ) ;
#3708 = DIRECTION ( 'NONE',  ( 0.2306359803922076457, 0.9730401042858025651, -1.412237191019970710E-17 ) ) ;
#3709 = CARTESIAN_POINT ( 'NONE',  ( 52.73786095581300515, -7.648876468381259564, -13.00000000000039968 ) ) ;
#3710 = ORIENTED_EDGE ( 'NONE', *, *, #12868, .F. ) ;
#3711 = VECTOR ( 'NONE', #17321, 1000.000000000000227 ) ;
#3712 = PLANE ( 'NONE',  #22067 ) ;
#3713 = CC_DESIGN_DATE_AND_TIME_ASSIGNMENT ( #18405, #16591, ( #9978 ) ) ;
#3714 = PRODUCT_DEFINITION ( 'UNKNOWN', '', #8383, #3733 ) ;
#3715 = ORIENTED_EDGE ( 'NONE', *, *, #7639, .F. ) ;
#3716 = DIRECTION ( 'NONE',  ( 0.2306359803922102825, 0.9730401042858017879, -4.163336342344335449E-15 ) ) ;
#3717 = DIRECTION ( 'NONE',  ( 0.000000000000000000, 1.020425574104004122E-16, 1.000000000000000000 ) ) ;
#3718 = AXIS2_PLACEMENT_3D ( 'NONE', #13774, #13883, #10105 ) ;
#3719 = ORIENTED_EDGE ( 'NONE', *, *, #2743, .F. ) ;
#3720 = EDGE_CURVE ( 'NONE', #10793, #989, #6541, .T. ) ;
#3721 = DIRECTION ( 'NONE',  ( -3.210834492181045054E-17, 2.441916418604790135E-15, 1.000000000000000000 ) ) ;
#3722 = EDGE_CURVE ( 'NONE', #12473, #489, #17542, .T. ) ;
#3723 = ORIENTED_EDGE ( 'NONE', *, *, #11766, .T. ) ;
#3724 = CC_DESIGN_PERSON_AND_ORGANIZATION_ASSIGNMENT ( #9987, #15534, ( #20495 ) ) ;
#3725 = LINE ( 'NONE', #9194, #13546 ) ;
#3726 = PERSON_AND_ORGANIZATION_ROLE ( 'creator' ) ;
#3727 = DIRECTION ( 'NONE',  ( 0.000000000000000000, 0.000000000000000000, 1.000000000000000000 ) ) ;
#3728 = CARTESIAN_POINT ( 'NONE',  ( -25.49859074735509878, -0.2321374729090530109, 2.500000000000000000 ) ) ;
#3729 =( NAMED_UNIT ( * ) SI_UNIT ( $, .STERADIAN. ) SOLID_ANGLE_UNIT ( ) );
#3730 = CARTESIAN_POINT ( 'NONE',  ( -65.62876257020761273, -24.89748912807110059, -5.000000000000000000 ) ) ;
#3731 = DIRECTION ( 'NONE',  ( 1.000000000000000000, 9.249025156865542385E-11, -2.269596547736322531E-13 ) ) ;
#3732 = DIRECTION ( 'NONE',  ( -0.005235963827108352890, 0.9999862922474493931, 5.936218956694023463E-19 ) ) ;
#3733 = DESIGN_CONTEXT ( 'detailed design', #8412, 'design' ) ;
#3734 = ADVANCED_FACE ( 'NONE', ( #20983, #19204, #6988 ), #14211, .T. ) ;
#3735 = FACE_OUTER_BOUND ( 'NONE', #9335, .T. ) ;
#3736 = CIRCLE ( 'NONE', #12798, 6.000000000001509015 ) ;
#3737 = CARTESIAN_POINT ( 'NONE',  ( 29.09552749756820234, -4.418411798633160359, 13.00000000000019895 ) ) ;
#3738 = CARTESIAN_POINT ( 'NONE',  ( 62.70840910389689782, 3.348031886875279639, 1.061114750357439988E-14 ) ) ;
#3739 = ORIENTED_EDGE ( 'NONE', *, *, #16968, .F. ) ;
#3740 = EDGE_CURVE ( 'NONE', #3048, #1063, #11442, .T. ) ;
#3741 = VERTEX_POINT ( 'NONE', #5178 ) ;
#3742 = DIRECTION ( 'NONE',  ( -0.9730401042858022320, 0.2306359803922080343, 5.959266323858941219E-17 ) ) ;
#3743 = DIRECTION ( 'NONE',  ( 1.159535895544890222E-14, 2.167612681253619929E-15, 1.000000000000000000 ) ) ;
#3744 = ORIENTED_EDGE ( 'NONE', *, *, #3021, .F. ) ;
#3745 = EDGE_CURVE ( 'NONE', #23097, #21187, #6627, .T. ) ;
#3746 = DIRECTION ( 'NONE',  ( 0.2306359803922095053, 0.9730401042858018990, 0.000000000000000000 ) ) ;
#3747 = ORIENTED_EDGE ( 'NONE', *, *, #18867, .T. ) ;
#3748 = EDGE_CURVE ( 'NONE', #8909, #2924, #18689, .T. ) ;
#3749 = DIRECTION ( 'NONE',  ( 1.000000000000000000, 0.000000000000000000, 0.000000000000000000 ) ) ;
#3750 = SECURITY_CLASSIFICATION_LEVEL ( 'unclassified' ) ;
#3751 = COORDINATED_UNIVERSAL_TIME_OFFSET ( 0, 0, .AHEAD. ) ;
#3752 = CARTESIAN_POINT ( 'NONE',  ( 33.16159828148069266, 10.35139963243406314, 26.29999999999999716 ) ) ;
#3753 = SECURITY_CLASSIFICATION ( '', '', #8005 ) ;
#3754 = DIRECTION ( 'NONE',  ( 0.9999862922474491711, 0.005235963827117207786, -1.514467536079854800E-31 ) ) ;
#3755 = VECTOR ( 'NONE', #18817, 1000.000000000000000 ) ;
#3756 = ORIENTED_EDGE ( 'NONE', *, *, #12062, .T. ) ;
#3757 = CARTESIAN_POINT ( 'NONE',  ( 31.45181451370270054, 16.90945435098589655, -23.00000000000000000 ) ) ;
#3758 = EDGE_LOOP ( 'NONE', ( #14593, #21185, #23005, #14005 ) ) ;
#3759 = CARTESIAN_POINT ( 'NONE',  ( 3.061616997868382648E-16, -2.500000000000000000, -5.000000000000000000 ) ) ;
#3760 = FACE_OUTER_BOUND ( 'NONE', #5998, .T. ) ;
#3761 = LINE ( 'NONE', #14694, #2702 ) ;
#3762 = ORIENTED_EDGE ( 'NONE', *, *, #4612, .F. ) ;
#3763 = APPROVAL_DATE_TIME ( #4010, #10397 ) ;
#3764 = FACE_OUTER_BOUND ( 'NONE', #16610, .T. ) ;
#3765 = EDGE_LOOP ( 'NONE', ( #7917, #14287, #16393, #6412 ) ) ;
#3766 = APPROVAL_STATUS ( 'not_yet_approved' ) ;
#3767 = ORIENTED_EDGE ( 'NONE', *, *, #18292, .F. ) ;
#3768 = VERTEX_POINT ( 'NONE', #279 ) ;
#3769 = LINE ( 'NONE', #11047, #18317 ) ;
#3770 = PERSON_AND_ORGANIZATION ( #11966, #8758 ) ;
#3771 = AXIS2_PLACEMENT_3D ( 'NONE', #2497, #16611, #13081 ) ;
#3772 = DIRECTION ( 'NONE',  ( 0.000000000000000000, 0.000000000000000000, -1.000000000000000000 ) ) ;
#3773 = APPROVAL_STATUS ( 'not_yet_approved' ) ;
#3774 = DIRECTION ( 'NONE',  ( -0.9730401042858035643, 0.2306359803922031215, -2.804983810440351899E-16 ) ) ;
#3775 = CIRCLE ( 'NONE', #21645, 0.2000000000000012046 ) ;
#3776 = ADVANCED_FACE ( 'NONE', ( #5411 ), #22016, .T. ) ;
#3777 = PLANE ( 'NONE',  #479 ) ;
#3778 = COORDINATED_UNIVERSAL_TIME_OFFSET ( 0, 0, .AHEAD. ) ;
#3779 = PRODUCT_DEFINITION_SHAPE ( 'NONE', 'NONE',  #23496 ) ;
#3780 = PRODUCT_DEFINITION_FORMATION_WITH_SPECIFIED_SOURCE ( 'ANY', '', #5117, .NOT_KNOWN. ) ;
#3781 = VERTEX_POINT ( 'NONE', #14782 ) ;
#3782 = AXIS2_PLACEMENT_3D ( 'NONE', #814, #12014, #8558 ) ;
#3783 = CARTESIAN_POINT ( 'NONE',  ( 28.14554285793940025, -3.006546890859610244, -15.00000000000039968 ) ) ;
#3784 = ORIENTED_EDGE ( 'NONE', *, *, #4549, .F. ) ;
#3785 = FACE_OUTER_BOUND ( 'NONE', #13387, .T. ) ;
#3786 = LINE ( 'NONE', #9504, #22901 ) ;
#3787 = FACE_BOUND ( 'NONE', #16674, .T. ) ;
#3788 = ORIENTED_EDGE ( 'NONE', *, *, #12033, .F. ) ;
#3789 = ORIENTED_EDGE ( 'NONE', *, *, #15619, .F. ) ;
#3790 = CARTESIAN_POINT ( 'NONE',  ( 117.0319250210129951, -13.02226701625849969, -15.90000000000000036 ) ) ;
#3791 = ORIENTED_EDGE ( 'NONE', *, *, #4675, .F. ) ;
#3792 = AXIS2_PLACEMENT_3D ( 'NONE', #10274, #11825, #17500 ) ;
#3793 = DATE_AND_TIME ( #5354, #3435 ) ;
#3794 = ORIENTED_EDGE ( 'NONE', *, *, #2974, .F. ) ;
#3795 = EDGE_LOOP ( 'NONE', ( #1365, #13169 ) ) ;
#3796 = FACE_OUTER_BOUND ( 'NONE', #12905, .T. ) ;
#3797 = CONICAL_SURFACE ( 'NONE', #4571, 5.386751345948120218, 1.047197551196598297 ) ;
#3798 = CARTESIAN_POINT ( 'NONE',  ( -20.22823963489775068, 17.95730124203003442, 5.000000000004473755 ) ) ;
#3799 = APPLICATION_PROTOCOL_DEFINITION ( 'international standard', 'config_control_design', 1994, #12343 ) ;
#3800 = APPLICATION_CONTEXT ( 'configuration controlled 3d designs of mechanical parts and assemblies' ) ;
#3801 = DIRECTION ( 'NONE',  ( 0.005235963827117092427, -0.9999862922474493931, -2.636227439667000721E-16 ) ) ;
#3802 = LOCAL_TIME ( 14, 11, 27.00000000000000000, #5478 ) ;
#3803 = DIRECTION ( 'NONE',  ( 0.9730401042858036753, -0.2306359803922031493, -5.432877459303553216E-17 ) ) ;
#3804 = APPROVAL_PERSON_ORGANIZATION ( #3506, #21194, #10778 ) ;
#3805 = ADVANCED_FACE ( 'NONE', ( #7092 ), #12673, .T. ) ;
#3806 =( NAMED_UNIT ( * ) SI_UNIT ( $, .STERADIAN. ) SOLID_ANGLE_UNIT ( ) );
#3807 = AXIS2_PLACEMENT_3D ( 'NONE', #902, #17307, #15042 ) ;
#3808 = CC_DESIGN_DATE_AND_TIME_ASSIGNMENT ( #4829, #15870, ( #4974 ) ) ;
#3809 = ORIENTED_EDGE ( 'NONE', *, *, #6903, .F. ) ;
#3810 = CARTESIAN_POINT ( 'NONE',  ( 33.27705887009660302, -3.036156860536619817, -13.00000000000000000 ) ) ;
#3811 = CALENDAR_DATE ( 2026, 31, 10 ) ;
#3812 =( BOUNDED_CURVE ( )  B_SPLINE_CURVE ( 2, ( #22358, #9567, #13124 ),
 .UNSPECIFIED., .F., .F. ) 
 B_SPLINE_CURVE_WITH_KNOTS ( ( 3, 3 ),
 ( 0.1168436138077928593, 0.2336872276155859962 ),
 .UNSPECIFIED. ) 
 CURVE ( )  GEOMETRIC_REPRESENTATION_ITEM ( )  RATIONAL_B_SPLINE_CURVE ( ( 1.077350269189624843, 1.077350269189625065, 1.000000000000000000 ) ) 
 REPRESENTATION_ITEM ( '' )  );
#3813 = VERTEX_POINT ( 'NONE', #16552 ) ;
#3814 = CARTESIAN_POINT ( 'NONE',  ( 29.36184298829670070, -3.294841866349740300, 11.00000000000019895 ) ) ;
#3815 = CARTESIAN_POINT ( 'NONE',  ( -69.90454993788389970, 6.134066389438220135, -0.7502499999999080460 ) ) ;
#3816 = ADVANCED_FACE ( 'NONE', ( #5637 ), #12564, .F. ) ;
#3817 = CLOSED_SHELL ( 'NONE', ( #17794, #8801, #17519, #16080, #5260, #9800, #21567, #15125, #13592, #6474, #17276, #5500, #12196, #15882, #23372, #19874, #1838, #1056, #7912, #3734 ) ) ;
#3818 = EDGE_CURVE ( 'NONE', #8021, #5959, #13017, .T. ) ;
#3819 = DIRECTION ( 'NONE',  ( -9.594916218540590128E-33, 2.583840697242805182E-16, -1.000000000000000000 ) ) ;
#3820 = LOCAL_TIME ( 14, 11, 27.00000000000000000, #11666 ) ;
#3821 = DIRECTION ( 'NONE',  ( 0.000000000000000000, 0.000000000000000000, -1.000000000000000000 ) ) ;
#3822 = CARTESIAN_POINT ( 'NONE',  ( 117.1011158151309957, -12.73035498497280038, -20.00000000000000000 ) ) ;
#3823 = APPROVAL_PERSON_ORGANIZATION ( #17040, #2102, #6123 ) ;
#3824 = ORIENTED_EDGE ( 'NONE', *, *, #412, .T. ) ;
#3825 = CARTESIAN_POINT ( 'NONE',  ( 113.4570673249340018, -28.10438863268850085, 3.399999999999999911 ) ) ;
#3826 = AXIS2_PLACEMENT_3D ( 'NONE', #20506, #9836, #13506 ) ;
#3827 = EDGE_LOOP ( 'NONE', ( #10553, #1774, #20650, #7900 ) ) ;
#3828 = ORIENTED_EDGE ( 'NONE', *, *, #16655, .T. ) ;
#3829 = DIRECTION ( 'NONE',  ( 1.159535895544890222E-14, 2.167612681253619929E-15, 1.000000000000000000 ) ) ;
#3830 = FACE_BOUND ( 'NONE', #19166, .T. ) ;
#3831 = SECURITY_CLASSIFICATION ( '', '', #7824 ) ;
#3832 = ORIENTED_EDGE ( 'NONE', *, *, #12843, .F. ) ;
#3833 = AXIS2_PLACEMENT_3D ( 'NONE', #876, #6108, #22137 ) ;
#3834 = CARTESIAN_POINT ( 'NONE',  ( -19.49999999982360066, -0.1021026942259700004, -2.500000000000000000 ) ) ;
#3835 = ORIENTED_EDGE ( 'NONE', *, *, #23276, .F. ) ;
#3836 = FACE_OUTER_BOUND ( 'NONE', #9931, .T. ) ;
#3837 = CARTESIAN_POINT ( 'NONE',  ( 42.82341786264430539, 18.59529084842194280, 12.99999999999970512 ) ) ;
#3838 = ADVANCED_FACE ( 'NONE', ( #5525 ), #2307, .F. ) ;
#3839 = CC_DESIGN_APPROVAL ( #17941, ( #6763 ) ) ;
#3840 = LOCAL_TIME ( 14, 11, 27.00000000000000000, #10047 ) ;
#3841 = DIRECTION ( 'NONE',  ( -0.9730401042858036753, 0.2306359803922028995, 5.958148513035547083E-17 ) ) ;
#3842 = CC_DESIGN_DATE_AND_TIME_ASSIGNMENT ( #19214, #1024, ( #5893 ) ) ;
#3843 = CARTESIAN_POINT ( 'NONE',  ( 40.42677426225490933, 27.12808637232345177, 12.99999999999979927 ) ) ;
#3844 = PERSON_AND_ORGANIZATION_ROLE ( 'design_supplier' ) ;
#3845 = CC_DESIGN_PERSON_AND_ORGANIZATION_ASSIGNMENT ( #1019, #11750, ( #14088 ) ) ;
#3846 = LOCAL_TIME ( 14, 11, 27.00000000000000000, #17902 ) ;
#3847 = DIRECTION ( 'NONE',  ( -0.4865200521429014491, 0.1153179901961012555, 0.8660254037844388186 ) ) ;
#3848 = DIRECTION ( 'NONE',  ( -0.9730401042858024541, 0.2306359803922080898, 5.959266323858592394E-17 ) ) ;
#3849 = EDGE_CURVE ( 'NONE', #13193, #18347, #3629, .T. ) ;
#3850 = EDGE_CURVE ( 'NONE', #11752, #23191, #1213, .T. ) ;
#3851 = CARTESIAN_POINT ( 'NONE',  ( -29.01760921662840076, 6.974057232812999274, -2.500000000000000000 ) ) ;
#3852 = CARTESIAN_POINT ( 'NONE',  ( -20.00000000000000000, -20.00000000000000000, 4.543842380125470691E-12 ) ) ;
#3853 = ADVANCED_FACE ( 'NONE', ( #23451 ), #18124, .T. ) ;
#3854 = EDGE_CURVE ( 'NONE', #3176, #20610, #1954, .T. ) ;
#3855 = FACE_OUTER_BOUND ( 'NONE', #6242, .T. ) ;
#3856 = DIRECTION ( 'NONE',  ( -2.270069654138870255E-15, -1.000000000000000000, -7.035747901516317327E-77 ) ) ;
#3857 = VERTEX_POINT ( 'NONE', #10790 ) ;
#3858 = LOCAL_TIME ( 14, 11, 27.00000000000000000, #10117 ) ;
#3859 = EDGE_LOOP ( 'NONE', ( #17470, #16589 ) ) ;
#3860 = DIRECTION ( 'NONE',  ( 0.9730401042858035643, -0.2306359803922028717, -5.959266323858674978E-17 ) ) ;
#3861 = CARTESIAN_POINT ( 'NONE',  ( -22.52506283708739687, 28.95208917575130414, -6.749999999995010214 ) ) ;
#3862 = VERTEX_POINT ( 'NONE', #3976 ) ;
#3863 = VECTOR ( 'NONE', #13706, 1000.000000000000000 ) ;
#3864 = CARTESIAN_POINT ( 'NONE',  ( 29.89447396975369742, -1.047702001782899961, 15.00000000000000000 ) ) ;
#3865 = ORIENTED_EDGE ( 'NONE', *, *, #19009, .F. ) ;
#3866 = VECTOR ( 'NONE', #15647, 1000.000000000000000 ) ;
#3867 = AXIS2_PLACEMENT_3D ( 'NONE', #13480, #14905, #8144 ) ;
#3868 = DIRECTION ( 'NONE',  ( 0.9999862922474493931, 0.005235963827108502076, 0.000000000000000000 ) ) ;
#3869 = CC_DESIGN_SECURITY_CLASSIFICATION ( #8052, ( #23505 ) ) ;
#3870 = COORDINATED_UNIVERSAL_TIME_OFFSET ( 0, 0, .AHEAD. ) ;
#3871 = CARTESIAN_POINT ( 'NONE',  ( 35.09747506357100377, 11.43410645592840069, -28.47000000000049980 ) ) ;
#3872 = CIRCLE ( 'NONE', #14876, 2.999999999999999556 ) ;
#3873 = EDGE_CURVE ( 'NONE', #15418, #4956, #12622, .T. ) ;
#3874 = PERSON_AND_ORGANIZATION_ROLE ( 'classification_officer' ) ;
#3875 = AXIS2_PLACEMENT_3D ( 'NONE', #4403, #9653, #470 ) ;
#3876 = EDGE_LOOP ( 'NONE', ( #1484, #13946, #15848, #14110 ) ) ;
#3877 = APPROVAL_PERSON_ORGANIZATION ( #10451, #12300, #2942 ) ;
#3878 = CARTESIAN_POINT ( 'NONE',  ( 34.89491389100820129, 23.30074776265919922, 13.00000000000000000 ) ) ;
#3879 = EDGE_LOOP ( 'NONE', ( #334, #20156 ) ) ;
#3880 = DIRECTION ( 'NONE',  ( 1.466984912809909902E-16, 2.805478249466310097E-20, 1.000000000000000000 ) ) ;
#3881 = EDGE_CURVE ( 'NONE', #10728, #19785, #3439, .T. ) ;
#3882 = AXIS2_PLACEMENT_3D ( 'NONE', #15257, #11723, #9577 ) ;
#3883 = EDGE_CURVE ( 'NONE', #21302, #20737, #2191, .T. ) ;
#3884 = VECTOR ( 'NONE', #10062, 1000.000000000000000 ) ;
#3885 = ORIENTED_EDGE ( 'NONE', *, *, #15434, .F. ) ;
#3886 = FACE_OUTER_BOUND ( 'NONE', #14180, .T. ) ;
#3887 = DIRECTION ( 'NONE',  ( -0.005235963827108231460, 0.9999862922474493931, 5.936218956694025389E-19 ) ) ;
#3888 = CARTESIAN_POINT ( 'NONE',  ( 38.09538026460416660, -1.352031289437040318, 13.00000000000000355 ) ) ;
#3889 = EDGE_LOOP ( 'NONE', ( #16454, #2382, #6661, #12524, #12318 ) ) ;
#3890 = CIRCLE ( 'NONE', #10752, 2.749999999999999112 ) ;
#3891 = PERSON_AND_ORGANIZATION_ROLE ( 'classification_officer' ) ;
#3892 = FACE_OUTER_BOUND ( 'NONE', #10247, .T. ) ;
#3893 = VECTOR ( 'NONE', #6366, 1000.000000000000114 ) ;
#3894 = ORIENTED_EDGE ( 'NONE', *, *, #4260, .F. ) ;
#3895 = VECTOR ( 'NONE', #14828, 1000.000000000000114 ) ;
#3896 = COORDINATED_UNIVERSAL_TIME_OFFSET ( 0, 0, .AHEAD. ) ;
#3897 = LOCAL_TIME ( 14, 11, 27.00000000000000000, #19795 ) ;
#3898 = VERTEX_POINT ( 'NONE', #21903 ) ;
#3899 = ORIENTED_EDGE ( 'NONE', *, *, #8544, .F. ) ;
#3900 = DIRECTION ( 'NONE',  ( -1.000000000000000000, -6.662112528310618598E-09, 2.269018306577664942E-13 ) ) ;
#3901 = APPROVAL_DATE_TIME ( #11048, #11152 ) ;
#3902 = VECTOR ( 'NONE', #10466, 1000.000000000000000 ) ;
#3903 = CIRCLE ( 'NONE', #13410, 2.499999999999999112 ) ;
#3904 = ADVANCED_FACE ( 'NONE', ( #9446 ), #22064, .F. ) ;
#3905 = VECTOR ( 'NONE', #12160, 999.9999999999998863 ) ;
#3906 = DIRECTION ( 'NONE',  ( 0.9730401042858035643, -0.2306359803922028717, -5.959266323858677443E-17 ) ) ;
#3907 = PERSON_AND_ORGANIZATION ( #7, #18191 ) ;
#3908 = CARTESIAN_POINT ( 'NONE',  ( -19.99999998251005806, -22.50000000000000000, 8.000000000004545697 ) ) ;
#3909 = EDGE_CURVE ( 'NONE', #8432, #9514, #11865, .T. ) ;
#3910 = SHAPE_REPRESENTATION_RELATIONSHIP ( 'NONE' , 'NONE' ,  #10862, #17868 ) ;
#3911 = EDGE_CURVE ( 'NONE', #3145, #184, #5337, .T. ) ;
#3913 = AXIS2_PLACEMENT_3D ( 'NONE', #5744, #3969, #387 ) ;
#3912 = DIRECTION ( 'NONE',  ( 0.005235963827121942714, -0.9999862922474493931, -2.738609489598291197E-14 ) ) ;
#3914 = CIRCLE ( 'NONE', #872, 3.499999999999998668 ) ;
#3915 = EDGE_CURVE ( 'NONE', #15256, #20661, #11095, .T. ) ;
#3916 = DATE_TIME_ROLE ( 'creation_date' ) ;
#3917 = LOCAL_TIME ( 14, 11, 27.00000000000000000, #10643 ) ;
#3918 = ORIENTED_EDGE ( 'NONE', *, *, #3171, .F. ) ;
#3919 = AXIS2_PLACEMENT_3D ( 'NONE', #9445, #7658, #14903 ) ;
#3920 = CARTESIAN_POINT ( 'NONE',  ( 43.81897180516431689, 0.03336243584794939404, -21.50000000000000000 ) ) ;
#3921 = ORIENTED_EDGE ( 'NONE', *, *, #1384, .T. ) ;
#3922 = AXIS2_PLACEMENT_3D ( 'NONE', #21270, #19271, #8469 ) ;
#3923 = PLANE ( 'NONE',  #12452 ) ;
#3924 = FACE_BOUND ( 'NONE', #1393, .T. ) ;
#3925 = DIRECTION ( 'NONE',  ( -3.099353312215989243E-62, 1.534091707905539548E-92, 1.000000000000000000 ) ) ;
#3926 = VERTEX_POINT ( 'NONE', #18365 ) ;
#3927 = ORIENTED_EDGE ( 'NONE', *, *, #8427, .T. ) ;
#3928 = DIRECTION ( 'NONE',  ( -0.9730401042858035643, 0.2306359803922028717, 5.958148513035547083E-17 ) ) ;
#3929 = ORIENTED_EDGE ( 'NONE', *, *, #413, .T. ) ;
#3930 = PERSON_AND_ORGANIZATION ( #11966, #8758 ) ;
#3931 = VERTEX_POINT ( 'NONE', #11831 ) ;
#3932 = ORIENTED_EDGE ( 'NONE', *, *, #22306, .F. ) ;
#3933 = DIRECTION ( 'NONE',  ( -0.7071067811865475727, 0.000000000000000000, -0.7071067811865475727 ) ) ;
#3934 = AXIS2_PLACEMENT_3D ( 'NONE', #7500, #14731, #21961 ) ;
#3935 = DIRECTION ( 'NONE',  ( 2.269747459788999852E-13, 2.220446049250325308E-15, 1.000000000000000000 ) ) ;
#3936 = DATE_TIME_ROLE ( 'classification_date' ) ;
#3937 = VECTOR ( 'NONE', #20155, 1000.000000000000114 ) ;
#3938 = CARTESIAN_POINT ( 'NONE',  ( 50.76434296088209663, 17.41090750189739822, -1.033499999999964336 ) ) ;
#3939 = CIRCLE ( 'NONE', #11570, 6.000000000000000000 ) ;
#3940 = APPROVAL ( #18469, 'UNSPECIFIED' ) ;
#3941 = EDGE_CURVE ( 'NONE', #17240, #10728, #14109, .T. ) ;
#3942 = ORIENTED_EDGE ( 'NONE', *, *, #4032, .T. ) ;
#3943 = DIRECTION ( 'NONE',  ( -0.9730401042858022320, 0.2306359803922080343, 5.959266323858941219E-17 ) ) ;
#3944 = PERSON_AND_ORGANIZATION ( #11966, #8758 ) ;
#3945 = VERTEX_POINT ( 'NONE', #9700 ) ;
#3946 = DIRECTION ( 'NONE',  ( 2.269747459789000104E-13, 2.220446049250330436E-15, 1.000000000000000000 ) ) ;
#3947 = CARTESIAN_POINT ( 'NONE',  ( 61.45890873801150178, 17.00438549795339682, 13.00000000000000000 ) ) ;
#3948 = DIRECTION ( 'NONE',  ( -1.000000000000000000, 2.275047181608927151E-16, 0.000000000000000000 ) ) ;
#3949 = AXIS2_PLACEMENT_3D ( 'NONE', #21656, #8975, #14661 ) ;
#3950 = CARTESIAN_POINT ( 'NONE',  ( 111.3370095633313070, 3.057699617097837219, 13.00000000000000000 ) ) ;
#3951 = FACE_BOUND ( 'NONE', #16971, .T. ) ;
#3952 = VERTEX_POINT ( 'NONE', #16915 ) ;
#3953 = CIRCLE ( 'NONE', #2826, 4.750000000000000000 ) ;
#3954 = DIRECTION ( 'NONE',  ( -0.2306359803922053697, -0.9730401042858028982, 0.000000000000000000 ) ) ;
#3955 = UNCERTAINTY_MEASURE_WITH_UNIT (LENGTH_MEASURE( 1.000000000000000082E-05 ), #5062, 'distance_accuracy_value', 'NONE');
#3956 = EDGE_CURVE ( 'NONE', #587, #4833, #636, .T. ) ;
#3957 = ORIENTED_EDGE ( 'NONE', *, *, #18643, .T. ) ;
#3958 = EDGE_LOOP ( 'NONE', ( #12760, #6293, #21946, #4189 ) ) ;
#3959 = DIRECTION ( 'NONE',  ( 0.000000000000000000, 0.000000000000000000, 1.000000000000000000 ) ) ;
#3960 = FACE_OUTER_BOUND ( 'NONE', #21181, .T. ) ;
#3961 = ORIENTED_EDGE ( 'NONE', *, *, #11411, .F. ) ;
#3962 = DIRECTION ( 'NONE',  ( 0.9999862922474493931, 0.005235963827108368503, 0.000000000000000000 ) ) ;
#3963 = ORIENTED_EDGE ( 'NONE', *, *, #12184, .T. ) ;
#3964 = DIRECTION ( 'NONE',  ( -0.9730401042858022320, 0.2306359803922080343, 5.959266323858941219E-17 ) ) ;
#3965 = APPROVAL_STATUS ( 'not_yet_approved' ) ;
#3966 = CARTESIAN_POINT ( 'NONE',  ( 34.67470932959380292, 24.53963568513870186, 11.00000000000000000 ) ) ;
#3967 = ADVANCED_FACE ( 'NONE', ( #15128 ), #2312, .F. ) ;
#3968 =( BOUNDED_CURVE ( )  B_SPLINE_CURVE ( 2, ( #627, #22487, #20353 ),
 .UNSPECIFIED., .F., .F. ) 
 B_SPLINE_CURVE_WITH_KNOTS ( ( 3, 3 ),
 ( 0.2928548593876180162, 0.5857097187752360323 ),
 .UNSPECIFIED. ) 
 CURVE ( )  GEOMETRIC_REPRESENTATION_ITEM ( )  RATIONAL_B_SPLINE_CURVE ( ( 1.000000000000000000, 1.037954849302059834, 1.000000000000000000 ) ) 
 REPRESENTATION_ITEM ( '' )  );
#3969 = DIRECTION ( 'NONE',  ( 0.2306359803922080620, 0.9730401042858023430, 5.073893018238627926E-14 ) ) ;
#3970 = FACE_OUTER_BOUND ( 'NONE', #10489, .T. ) ;
#3971 = COORDINATED_UNIVERSAL_TIME_OFFSET ( 0, 0, .AHEAD. ) ;
#3972 = LINE ( 'NONE', #19286, #21396 ) ;
#3973 = DIRECTION ( 'NONE',  ( 0.005235964011423952132, -0.9999862922464843873, 2.442051063554900023E-15 ) ) ;
#3974 = DIRECTION ( 'NONE',  ( 5.039851780001396616E-28, 2.220446049301850153E-15, 1.000000000000000000 ) ) ;
#3975 = CARTESIAN_POINT ( 'NONE',  ( -25.64168762722610140, 6.365828311191160438, -5.000000000000000000 ) ) ;
#3976 = CARTESIAN_POINT ( 'NONE',  ( 36.78282996199610722, 11.03463321983559986, -27.69000000000049866 ) ) ;
#3977 = EDGE_LOOP ( 'NONE', ( #16493, #18923, #18510, #7046 ) ) ;
#3978 = ADVANCED_BREP_SHAPE_REPRESENTATION ( '', ( #17139, #12739 ), #19550 ) ;
#3979 = EDGE_CURVE ( 'NONE', #7239, #8426, #15015, .T. ) ;
#3980 = VECTOR ( 'NONE', #18526, 999.9999999999998863 ) ;
#3981 = ORIENTED_EDGE ( 'NONE', *, *, #4300, .F. ) ;
#3982 = DIRECTION ( 'NONE',  ( -2.269747459788994803E-13, -2.220446049250320181E-15, -1.000000000000000000 ) ) ;
#3983 = CARTESIAN_POINT ( 'NONE',  ( -0.5391976746803449627, 18.33937061236850141, -7.621247264287879719E-15 ) ) ;
#3984 = EDGE_LOOP ( 'NONE', ( #10242, #4174 ) ) ;
#3985 = CC_DESIGN_DATE_AND_TIME_ASSIGNMENT ( #5332, #13064, ( #11759 ) ) ;
#3986 = DIRECTION ( 'NONE',  ( -0.9730401042858036753, 0.2306359803922028995, 5.959266323858677443E-17 ) ) ;
#3987 = EDGE_LOOP ( 'NONE', ( #9039, #12941 ) ) ;
#3988 = CC_DESIGN_DATE_AND_TIME_ASSIGNMENT ( #8991, #10794, ( #9939 ) ) ;
#3989 = FACE_OUTER_BOUND ( 'NONE', #13509, .T. ) ;
#3990 = CALENDAR_DATE ( 2026, 31, 10 ) ;
#3991 = CARTESIAN_POINT ( 'NONE',  ( -23.50000000000000000, -20.00000000000000000, -2.500000000000000000 ) ) ;
#3992 = ADVANCED_FACE ( 'NONE', ( #4096 ), #10056, .T. ) ;
#3993 = EDGE_CURVE ( 'NONE', #1846, #3168, #6110, .T. ) ;
#3994 = PRODUCT_DEFINITION_SHAPE ( 'NONE', 'NONE',  #23493 ) ;
#3995 = SECURITY_CLASSIFICATION_LEVEL ( 'unclassified' ) ;
#3996 = APPLICATION_CONTEXT ( 'configuration controlled 3d designs of mechanical parts and assemblies' ) ;
#3997 = PLANE ( 'NONE',  #21918 ) ;
#3998 = EDGE_LOOP ( 'NONE', ( #22727, #15161, #8226, #7577 ) ) ;
#3999 = AXIS2_PLACEMENT_3D ( 'NONE', #2714, #66, #7447 ) ;
#4000 = CARTESIAN_POINT ( 'NONE',  ( 49.97703550743810297, 19.72589006658010291, 13.00000000000000000 ) ) ;
#4001 = EDGE_LOOP ( 'NONE', ( #16150, #4133, #21391, #19693, #11776 ) ) ;
#4002 = CARTESIAN_POINT ( 'NONE',  ( -25.49859074735509878, -0.2321374729090499855, 3.750000000000000000 ) ) ;
#4003 = DIRECTION ( 'NONE',  ( -0.9999862922474492821, -0.005235963827108258348, 0.000000000000000000 ) ) ;
#4004 = ORIENTED_EDGE ( 'NONE', *, *, #6613, .F. ) ;
#4005 = DIRECTION ( 'NONE',  ( 0.000000000000000000, 0.000000000000000000, -1.000000000000000000 ) ) ;
#4006 = DIRECTION ( 'NONE',  ( -2.656137997592320068E-16, 6.783012436524469908E-17, 1.000000000000000000 ) ) ;
#4007 = DIRECTION ( 'NONE',  ( 0.2306359803922033713, 0.9730401042858034533, -4.558064749665356219E-15 ) ) ;
#4008 = ORIENTED_EDGE ( 'NONE', *, *, #11481, .T. ) ;
#4009 = EDGE_CURVE ( 'NONE', #14240, #9157, #17912, .T. ) ;
#4010 = DATE_AND_TIME ( #21817, #13376 ) ;
#4011 = DIRECTION ( 'NONE',  ( 2.269881297312570136E-47, 1.000000000000000000, -2.269881297312570136E-47 ) ) ;
#4012 = ORIENTED_EDGE ( 'NONE', *, *, #20853, .F. ) ;
#4014 = APPROVAL_ROLE ( '' ) ;
#4013 = APPROVAL ( #7131, 'UNSPECIFIED' ) ;
#4015 = DIRECTION ( 'NONE',  ( 3.210834492194360164E-17, -2.441916418604790135E-15, -1.000000000000000000 ) ) ;
#4016 = ORIENTED_EDGE ( 'NONE', *, *, #22281, .F. ) ;
#4017 =( GEOMETRIC_REPRESENTATION_CONTEXT ( 3 ) GLOBAL_UNCERTAINTY_ASSIGNED_CONTEXT ( ( #19409 ) ) GLOBAL_UNIT_ASSIGNED_CONTEXT ( ( #12292, #19623, #15829 ) ) REPRESENTATION_CONTEXT ( 'NONE', 'WORKASPACE' ) );
#4018 = ORIENTED_EDGE ( 'NONE', *, *, #11258, .T. ) ;
#4019 = CC_DESIGN_PERSON_AND_ORGANIZATION_ASSIGNMENT ( #19160, #6567, ( #22291 ) ) ;
#4020 = CARTESIAN_POINT ( 'NONE',  ( 37.37362508103680625, 25.08661566644159890, 13.00000000000000000 ) ) ;
#4021 = COORDINATED_UNIVERSAL_TIME_OFFSET ( 0, 0, .AHEAD. ) ;
#4022 = ADVANCED_FACE ( 'NONE', ( #2444 ), #6348, .F. ) ;
#4023 = EDGE_CURVE ( 'NONE', #6518, #18157, #16762, .T. ) ;
#4024 = AXIS2_PLACEMENT_3D ( 'NONE', #22243, #17025, #18721 ) ;
#4025 = LINE ( 'NONE', #5816, #14226 ) ;
#4026 = DIRECTION ( 'NONE',  ( 0.000000000000000000, -2.710505431696529444E-14, 1.000000000000000000 ) ) ;
#4027 = CALENDAR_DATE ( 2026, 31, 10 ) ;
#4028 = VECTOR ( 'NONE', #20942, 1000.000000000000000 ) ;
#4029 = ORIENTED_EDGE ( 'NONE', *, *, #816, .F. ) ;
#4030 = CARTESIAN_POINT ( 'NONE',  ( 111.3370095633313070, 3.057699617097787037, -13.00000000000000000 ) ) ;
#4031 = ORIENTED_EDGE ( 'NONE', *, *, #7331, .F. ) ;
#4032 = EDGE_CURVE ( 'NONE', #2950, #7235, #3890, .T. ) ;
#4033 = DIRECTION ( 'NONE',  ( 0.005235963827117092427, -0.9999862922474493931, -2.636227439667000721E-16 ) ) ;
#4034 = DIRECTION ( 'NONE',  ( -0.9730401042858036753, 0.2306359803922028995, 5.959266323858677443E-17 ) ) ;
#4035 = CARTESIAN_POINT ( 'NONE',  ( 43.45766680872284837, 21.27115113520789791, 12.99999999999970157 ) ) ;
#4036 = ORIENTED_EDGE ( 'NONE', *, *, #21028, .F. ) ;
#4037 = EDGE_LOOP ( 'NONE', ( #2734, #6715, #5931, #12250 ) ) ;
#4038 = DIRECTION ( 'NONE',  ( -0.9730401042858022320, 0.2306359803922080343, 5.959266323858951079E-17 ) ) ;
#4039 = VERTEX_POINT ( 'NONE', #745 ) ;
#4040 = PERSON_AND_ORGANIZATION_ROLE ( 'creator' ) ;
#4041 = EDGE_CURVE ( 'NONE', #20805, #8421, #13129, .T. ) ;
#4042 = ORIENTED_EDGE ( 'NONE', *, *, #15951, .T. ) ;
#4043 = ORIENTED_EDGE ( 'NONE', *, *, #19061, .F. ) ;
#4044 = DIRECTION ( 'NONE',  ( -1.000000000000000000, 0.000000000000000000, 0.000000000000000000 ) ) ;
#4045 = SPHERICAL_SURFACE ( 'NONE', #3600, 15.25000000000000000 ) ;
#4046 = DATE_TIME_ROLE ( 'creation_date' ) ;
#4047 = ADVANCED_FACE ( 'NONE', ( #11720 ), #20479, .F. ) ;
#4048 = FACE_OUTER_BOUND ( 'NONE', #10203, .T. ) ;
#4049 = CONICAL_SURFACE ( 'NONE', #17328, 2.283499999999998753, 0.7853981633974433940 ) ;
#4050 = EDGE_CURVE ( 'NONE', #23466, #290, #4344, .T. ) ;
#4051 = DIRECTION ( 'NONE',  ( 0.000000000000000000, -2.739767185169682068E-14, 1.000000000000000000 ) ) ;
#4052 = CIRCLE ( 'NONE', #17329, 2.500000000000000000 ) ;
#4053 = CIRCLE ( 'NONE', #17729, 2.009240000000000581 ) ;
#4054 = ORIENTED_EDGE ( 'NONE', *, *, #14710, .F. ) ;
#4055 = LINE ( 'NONE', #6068, #5249 ) ;
#4056 = PERSON_AND_ORGANIZATION_ROLE ( 'design_owner' ) ;
#4057 = ORIENTED_EDGE ( 'NONE', *, *, #8962, .T. ) ;
#4058 = VECTOR ( 'NONE', #17856, 1000.000000000000227 ) ;
#4059 = CARTESIAN_POINT ( 'NONE',  ( -26.26776695296636888, -30.47499999999999432, 20.76776695296636888 ) ) ;
#4060 = DIRECTION ( 'NONE',  ( -8.326672684687908612E-17, -1.000000000000000000, 1.564125491189519930E-30 ) ) ;
#4061 = VECTOR ( 'NONE', #12054, 1000.000000000000000 ) ;
#4062 = CARTESIAN_POINT ( 'NONE',  ( -19.55420733641118147, 2.397309549614573765, -5.000000000000006217 ) ) ;
#4063 = VECTOR ( 'NONE', #11196, 999.9999999999998863 ) ;
#4064 = CARTESIAN_POINT ( 'NONE',  ( -30.75845054331819739, -0.1610523420890279944, -2.999000000000079602 ) ) ;
#4065 = ORIENTED_EDGE ( 'NONE', *, *, #10833, .T. ) ;
#4066 = DIRECTION ( 'NONE',  ( -0.9730401042858035643, 0.2306359803922028717, -2.804983810440358308E-16 ) ) ;
#4067 = APPROVAL ( #16145, 'UNSPECIFIED' ) ;
#4068 = SHAPE_DEFINITION_REPRESENTATION ( #16116, #7508 ) ;
#4069 = EDGE_CURVE ( 'NONE', #115, #12698, #18726, .T. ) ;
#4070 = ORIENTED_EDGE ( 'NONE', *, *, #16465, .F. ) ;
#4071 = ORIENTED_EDGE ( 'NONE', *, *, #12962, .T. ) ;
#4072 = PLANE ( 'NONE',  #1623 ) ;
#4073 = CARTESIAN_POINT ( 'NONE',  ( 31.11077410011089839, -1.335996977273280262, -11.00000000000039968 ) ) ;
#4074 = AXIS2_PLACEMENT_3D ( 'NONE', #18580, #19996, #16783 ) ;
#4075 = EDGE_LOOP ( 'NONE', ( #5321, #7486, #5780, #19354 ) ) ;
#4076 = PERSON_AND_ORGANIZATION ( #11966, #8758 ) ;
#4077 = DIRECTION ( 'NONE',  ( -0.9730401042858022320, 0.2306359803922080343, -1.978423856035325353E-31 ) ) ;
#4078 = CARTESIAN_POINT ( 'NONE',  ( 31.45181451370270054, 16.90945435098589655, -23.00000000000000000 ) ) ;
#4079 = CIRCLE ( 'NONE', #17361, 2.499999999999999112 ) ;
#4080 = COORDINATED_UNIVERSAL_TIME_OFFSET ( 0, 0, .AHEAD. ) ;
#4081 = DIRECTION ( 'NONE',  ( 0.000000000000000000, 1.668003342285391304E-16, 1.000000000000000000 ) ) ;
#4082 = CONICAL_SURFACE ( 'NONE', #14321, 2.693275000000006081, 0.7853166638051269910 ) ;
#4083 = AXIS2_PLACEMENT_3D ( 'NONE', #9795, #8352, #21056 ) ;
#4084 =( NAMED_UNIT ( * ) PLANE_ANGLE_UNIT ( ) SI_UNIT ( $, .RADIAN. ) );
#4085 = DIRECTION ( 'NONE',  ( 0.005235963827121941846, -0.9999862922474492821, -5.936218956657112052E-19 ) ) ;
#4086 = EDGE_CURVE ( 'NONE', #9241, #12615, #15253, .T. ) ;
#4087 = DIRECTION ( 'NONE',  ( -1.000000000000000000, 0.000000000000000000, 0.000000000000000000 ) ) ;
#4088 = APPROVAL_ROLE ( '' ) ;
#4089 = DIRECTION ( 'NONE',  ( -0.9730401042858024541, 0.2306359803922080898, 5.959266323853292235E-17 ) ) ;
#4090 = AXIS2_PLACEMENT_3D ( 'NONE', #18249, #13028, #9585 ) ;
#4091 = FACE_OUTER_BOUND ( 'NONE', #2318, .T. ) ;
#4092 = DIRECTION ( 'NONE',  ( -0.9730401042858035643, 0.2306359803922028717, 5.958148513035547083E-17 ) ) ;
#4093 = CARTESIAN_POINT ( 'NONE',  ( -60.06514239919540188, -6.814592325618320068, -5.500000000000079048 ) ) ;
#4094 = AXIS2_PLACEMENT_3D ( 'NONE', #9594, #11626, #2459 ) ;
#4095 = DIRECTION ( 'NONE',  ( 2.982858504577324546E-17, -2.441916418604795262E-15, -1.000000000000000000 ) ) ;
#4096 = FACE_OUTER_BOUND ( 'NONE', #6552, .T. ) ;
#4097 = ORIENTED_EDGE ( 'NONE', *, *, #6692, .F. ) ;
#4098 = VECTOR ( 'NONE', #20359, 999.9999999999998863 ) ;
#4099 = ORIENTED_EDGE ( 'NONE', *, *, #6330, .F. ) ;
#4100 = DIRECTION ( 'NONE',  ( -6.574470837186350421E-32, 2.286959927910970108E-15, 1.000000000000000000 ) ) ;
#4101 = AXIS2_PLACEMENT_3D ( 'NONE', #19515, #16629, #20560 ) ;
#4102 = DIRECTION ( 'NONE',  ( -0.9999862922474492821, -0.005235963827121951387, 1.466966272682004590E-16 ) ) ;
#4103 = VERTEX_POINT ( 'NONE', #18941 ) ;
#4104 = CYLINDRICAL_SURFACE ( 'NONE', #12272, 7.000000000000000888 ) ;
#4105 = ORIENTED_EDGE ( 'NONE', *, *, #8140, .F. ) ;
#4106 = DIRECTION ( 'NONE',  ( -1.138590270679730064E-14, -2.220446049251240387E-15, -1.000000000000000000 ) ) ;
#4107 = COORDINATED_UNIVERSAL_TIME_OFFSET ( 0, 0, .AHEAD. ) ;
#4108 = CARTESIAN_POINT ( 'NONE',  ( -65.80336369117380002, 8.448563927732790191, -5.000000000000000000 ) ) ;
#4109 = PERSON_AND_ORGANIZATION_ROLE ( 'classification_officer' ) ;
#4110 = CARTESIAN_POINT ( 'NONE',  ( -22.50000000000000000, -20.00000001665527805, 6.750000000004588330 ) ) ;
#4111 = ORIENTED_EDGE ( 'NONE', *, *, #7073, .T. ) ;
#4112 = EDGE_CURVE ( 'NONE', #7324, #22882, #7659, .T. ) ;
#4113 = VECTOR ( 'NONE', #2336, 1000.000000000000000 ) ;
#4114 = LINE ( 'NONE', #14930, #9248 ) ;
#4115 = VERTEX_POINT ( 'NONE', #17156 ) ;
#4116 = CARTESIAN_POINT ( 'NONE',  ( 0.000000000000000000, -17.30000000000000071, -5.000000000000000000 ) ) ;
#4117 = APPROVAL ( #17680, 'UNKNOWN' ) ;
#4118 = DIRECTION ( 'NONE',  ( -0.04564792618501069266, -0.9989575901083128651, 2.775557561562892534E-15 ) ) ;
#4119 = VERTEX_POINT ( 'NONE', #20365 ) ;
#4120 = CARTESIAN_POINT ( 'NONE',  ( 35.59419854219520118, 9.774809681453540122, 26.30000000000000071 ) ) ;
#4121 = PLANE ( 'NONE',  #5765 ) ;
#4122 = CARTESIAN_POINT ( 'NONE',  ( 34.67470932959370344, 24.53963568513860238, -15.00000000000049916 ) ) ;
#4123 = ORIENTED_EDGE ( 'NONE', *, *, #1084, .F. ) ;
#4124 =( REPRESENTATION_RELATIONSHIP ('NONE','NONE', #19303, #13540 ) REPRESENTATION_RELATIONSHIP_WITH_TRANSFORMATION ( #13849 )SHAPE_REPRESENTATION_RELATIONSHIP( ) );
#4125 = EDGE_CURVE ( 'NONE', #18347, #2417, #3522, .T. ) ;
#4126 = ADVANCED_FACE ( 'NONE', ( #13709 ), #10411, .T. ) ;
#4127 = DATE_AND_TIME ( #11281, #4641 ) ;
#4128 = DIRECTION ( 'NONE',  ( 0.000000000000000000, 1.000000000000000000, 0.000000000000000000 ) ) ;
#4129 = ORIENTED_EDGE ( 'NONE', *, *, #2167, .F. ) ;
#4130 = APPROVAL_DATE_TIME ( #5913, #20272 ) ;
#4131 = FACE_OUTER_BOUND ( 'NONE', #11927, .T. ) ;
#4132 = ORIENTED_EDGE ( 'NONE', *, *, #21558, .F. ) ;
#4133 = ORIENTED_EDGE ( 'NONE', *, *, #19138, .T. ) ;
#4134 = DIRECTION ( 'NONE',  ( 0.9730401042858046745, -0.2306359803921981810, 0.000000000000000000 ) ) ;
#4135 = SHAPE_DEFINITION_REPRESENTATION ( #18992, #12659 ) ;
#4136 = APPROVAL_ROLE ( '' ) ;
#4137 = CARTESIAN_POINT ( 'NONE',  ( -20.00000000000149925, -20.00000000000000000, 8.750000000004709122 ) ) ;
#4138 = VECTOR ( 'NONE', #7903, 1000.000000000000114 ) ;
#4139 = EDGE_CURVE ( 'NONE', #1257, #16889, #19525, .T. ) ;
#4140 = FACE_OUTER_BOUND ( 'NONE', #19965, .T. ) ;
#4141 = CC_DESIGN_PERSON_AND_ORGANIZATION_ASSIGNMENT ( #11020, #23235, ( #7796 ) ) ;
#4142 = PERSON_AND_ORGANIZATION ( #11966, #8758 ) ;
#4143 = CC_DESIGN_PERSON_AND_ORGANIZATION_ASSIGNMENT ( #1375, #18974, ( #9559 ) ) ;
#4144 = EDGE_LOOP ( 'NONE', ( #15314, #21126, #15377, #16738 ) ) ;
#4145 = DIRECTION ( 'NONE',  ( -1.000000000000000000, -6.662111466122900240E-09, 1.138590272159020020E-14 ) ) ;
#4146 = ORIENTED_EDGE ( 'NONE', *, *, #10459, .F. ) ;
#4147 = EDGE_CURVE ( 'NONE', #20385, #3524, #19408, .T. ) ;
#4148 = EDGE_CURVE ( 'NONE', #1957, #12690, #1611, .T. ) ;
#4149 = FACE_OUTER_BOUND ( 'NONE', #14057, .T. ) ;
#4150 = PRODUCT_RELATED_PRODUCT_CATEGORY ( 'detail', '', ( #1697 ) ) ;
#4151 = PLANE ( 'NONE',  #13055 ) ;
#4152 = CARTESIAN_POINT ( 'NONE',  ( -58.58222095029707077, 7.653029331589754847, 2.499999999999999556 ) ) ;
#4153 = EDGE_LOOP ( 'NONE', ( #3182, #401, #18884, #12847 ) ) ;
#4154 = VECTOR ( 'NONE', #1915, 1000.000000000000000 ) ;
#4155 = ORIENTED_EDGE ( 'NONE', *, *, #5195, .F. ) ;
#4156 = ADVANCED_FACE ( 'NONE', ( #17398 ), #6825, .T. ) ;
#4158 = DIRECTION ( 'NONE',  ( -0.9997651245102160411, -0.02167246670483410909, 0.000000000000000000 ) ) ;
#4157 = AXIS2_PLACEMENT_3D ( 'NONE', #15111, #9788, #14880 ) ;
#4159 = ORIENTED_EDGE ( 'NONE', *, *, #6668, .T. ) ;
#4160 = PERSON_AND_ORGANIZATION ( #11966, #8758 ) ;
#4161 = ORIENTED_EDGE ( 'NONE', *, *, #11974, .F. ) ;
#4162 = ORIENTED_EDGE ( 'NONE', *, *, #19946, .T. ) ;
#4163 = CARTESIAN_POINT ( 'NONE',  ( -18.05391955182270181, 22.49081825942809942, -4.900728725074969882E-15 ) ) ;
#4164 = CARTESIAN_POINT ( 'NONE',  ( 35.89100945995100034, 24.25134070964849897, 15.00000000000000000 ) ) ;
#4165 = APPROVAL_ROLE ( '' ) ;
#4166 = CARTESIAN_POINT ( 'NONE',  ( 113.2033677465029911, -29.17473274740279976, 13.00000000000000000 ) ) ;
#4167 = CARTESIAN_POINT ( 'NONE',  ( 36.89121352362748496, 22.27682603178741516, 11.00000000000000000 ) ) ;
#4168 = EDGE_CURVE ( 'NONE', #17440, #4537, #17636, .T. ) ;
#4169 = DIRECTION ( 'NONE',  ( 0.000000000000000000, 0.000000000000000000, 1.000000000000000000 ) ) ;
#4170 = AXIS2_PLACEMENT_3D ( 'NONE', #13432, #3928, #16860 ) ;
#4171 = ORIENTED_EDGE ( 'NONE', *, *, #13106, .T. ) ;
#4172 = DIRECTION ( 'NONE',  ( 3.210834492194344756E-17, -2.441916418604790135E-15, -1.000000000000000000 ) ) ;
#4173 = COORDINATED_UNIVERSAL_TIME_OFFSET ( 0, 0, .AHEAD. ) ;
#4174 = ORIENTED_EDGE ( 'NONE', *, *, #12693, .T. ) ;
#4175 = CARTESIAN_POINT ( 'NONE',  ( 58.28050119523756933, -0.7409723595832931053, 3.718515598612927419E-14 ) ) ;
#4176 = DIRECTION ( 'NONE',  ( 1.000000000000000000, 3.099353312215988811E-62, 0.000000000000000000 ) ) ;
#4177 = AXIS2_PLACEMENT_3D ( 'NONE', #23301, #8947, #135 ) ;
#4178 = ORIENTED_EDGE ( 'NONE', *, *, #16477, .T. ) ;
#4179 = EDGE_CURVE ( 'NONE', #23086, #16983, #19830, .T. ) ;
#4180 = CARTESIAN_POINT ( 'NONE',  ( 30.84445860938240003, -2.459566909556569758, 17.25000000000019895 ) ) ;
#4181 = EDGE_CURVE ( 'NONE', #16628, #15219, #17172, .T. ) ;
#4182 = DIRECTION ( 'NONE',  ( -0.9999862922474492821, -0.005235963827121951387, 1.239088197126291310E-16 ) ) ;
#4183 = ORIENTED_EDGE ( 'NONE', *, *, #11972, .F. ) ;
#4184 = CARTESIAN_POINT ( 'NONE',  ( -68.71210320717760567, 12.64039918458589895, 4.433884350144319916E-15 ) ) ;
#4185 = DATE_AND_TIME ( #6215, #10278 ) ;
#4186 = PRODUCT_DEFINITION_SHAPE ( 'NONE', 'NONE',  #23482 ) ;
#4187 = LOCAL_TIME ( 14, 11, 27.00000000000000000, #7253 ) ;
#4188 = EDGE_LOOP ( 'NONE', ( #7620, #21259, #10987, #15430, #6888 ) ) ;
#4189 = ORIENTED_EDGE ( 'NONE', *, *, #16476, .F. ) ;
#4190 = DIRECTION ( 'NONE',  ( 0.2306359803922028995, 0.9730401042858036753, -9.756037151021835575E-16 ) ) ;
#4191 = DIRECTION ( 'NONE',  ( 3.211814849206744928E-17, -2.442368445299930211E-15, -1.000000000000000000 ) ) ;
#4192 = AXIS2_PLACEMENT_3D ( 'NONE', #19196, #17300, #571 ) ;
#4193 = ORIENTED_EDGE ( 'NONE', *, *, #7973, .T. ) ;
#4194 = COORDINATED_UNIVERSAL_TIME_OFFSET ( 0, 0, .AHEAD. ) ;
#4195 = CARTESIAN_POINT ( 'NONE',  ( -3.499952022866071211, -0.01832587339492760051, -8.848002871973867878E-14 ) ) ;
#4196 = CARTESIAN_POINT ( 'NONE',  ( -28.52462712253550237, 6.350733138482030249, 0.7325259402521719920 ) ) ;
#4197 = COORDINATED_UNIVERSAL_TIME_OFFSET ( 0, 0, .AHEAD. ) ;
#4198 = DIRECTION ( 'NONE',  ( -1.000000000000000000, 2.775557561562891351E-15, 0.000000000000000000 ) ) ;
#4199 = AXIS2_PLACEMENT_3D ( 'NONE', #2868, #14933, #3443 ) ;
#4200 = DIRECTION ( 'NONE',  ( 0.000000000000000000, 0.000000000000000000, 1.000000000000000000 ) ) ;
#4201 = DIRECTION ( 'NONE',  ( 1.040345436475888435E-32, 1.169424102322700040E-16, 1.000000000000000000 ) ) ;
#4202 = CALENDAR_DATE ( 2026, 31, 10 ) ;
#4203 = LOCAL_TIME ( 14, 11, 27.00000000000000000, #17723 ) ;
#4204 = EDGE_CURVE ( 'NONE', #14607, #10212, #15662, .T. ) ;
#4205 = APPROVAL_PERSON_ORGANIZATION ( #18716, #1881, #13003 ) ;
#4206 = LINE ( 'NONE', #9803, #10423 ) ;
#4207 = DIRECTION ( 'NONE',  ( -0.9730401042858036753, 0.2306359803922031493, -2.740969466505752002E-16 ) ) ;
#4208 = ADVANCED_FACE ( 'NONE', ( #10283 ), #15727, .T. ) ;
#4210 = DIRECTION ( 'NONE',  ( -0.8823529412199658806, 0.4705882352125641543, 1.991462550421374292E-13 ) ) ;
#4209 = AXIS2_PLACEMENT_3D ( 'NONE', #22525, #905, #6493 ) ;
#4211 = CARTESIAN_POINT ( 'NONE',  ( 31.01827548281339020, -2.500766059351007708, 11.00000000000020428 ) ) ;
#4212 = CC_DESIGN_APPROVAL ( #13695, ( #4974 ) ) ;
#4213 = CARTESIAN_POINT ( 'NONE',  ( -19.99995718853209681, 22.95166395734829834, 2.499999999999950262 ) ) ;
#4214 = DIRECTION ( 'NONE',  ( -2.269700743865584947E-13, -2.220446049247695246E-15, -1.000000000000000000 ) ) ;
#4215 = AXIS2_PLACEMENT_3D ( 'NONE', #20256, #3626, #10899 ) ;
#4216 = VERTEX_POINT ( 'NONE', #14058 ) ;
#4217 = EDGE_LOOP ( 'NONE', ( #21612, #14236, #4920, #17701 ) ) ;
#4218 = LINE ( 'NONE', #13485, #18709 ) ;
#4219 = CARTESIAN_POINT ( 'NONE',  ( 35.34725016111838869, 18.05499787358318287, 12.99999999999979927 ) ) ;
#4220 = EDGE_LOOP ( 'NONE', ( #4161, #17253 ) ) ;
#4221 = CARTESIAN_POINT ( 'NONE',  ( -29.94686441333699989, 7.343408934390589948, 3.750000000000000000 ) ) ;
#4222 = ORIENTED_EDGE ( 'NONE', *, *, #15354, .F. ) ;
#4223 = CC_DESIGN_APPROVAL ( #19543, ( #6875 ) ) ;
#4224 = DIRECTION ( 'NONE',  ( -0.9730401042858035643, 0.2306359803922028717, 5.667427308550587516E-17 ) ) ;
#4225 = PRODUCT_DEFINITION_FORMATION_WITH_SPECIFIED_SOURCE ( 'ANY', '', #12718, .NOT_KNOWN. ) ;
#4226 = PERSON_AND_ORGANIZATION ( #11966, #8758 ) ;
#4227 = AXIS2_PLACEMENT_3D ( 'NONE', #15312, #4852, #4622 ) ;
#4228 = FACE_OUTER_BOUND ( 'NONE', #21178, .T. ) ;
#4229 = CC_DESIGN_APPROVAL ( #14439, ( #9926 ) ) ;
#4230 = DIRECTION ( 'NONE',  ( 1.000000000000000000, -6.281952996264290168E-17, 3.503246160812045303E-47 ) ) ;
#4231 = PRODUCT_DEFINITION ( 'UNKNOWN', '', #8384, #20338 ) ;
#4232 = ORIENTED_EDGE ( 'NONE', *, *, #15770, .T. ) ;
#4233 = DIRECTION ( 'NONE',  ( 1.000000000000000000, 0.000000000000000000, 0.000000000000000000 ) ) ;
#4234 = EDGE_LOOP ( 'NONE', ( #5357, #22758, #13263, #4953 ) ) ;
#4235 = CARTESIAN_POINT ( 'NONE',  ( -30.79248430819469817, 6.338858557518999959, -5.500000000000089706 ) ) ;
#4236 = LOCAL_TIME ( 14, 11, 27.00000000000000000, #10555 ) ;
#4237 = CARTESIAN_POINT ( 'NONE',  ( 36.09092202081949807, 8.115512906978459284, 27.68999999999999773 ) ) ;
#4238 = ORIENTED_EDGE ( 'NONE', *, *, #20669, .T. ) ;
#4239 = CARTESIAN_POINT ( 'NONE',  ( 37.65360996504041680, 27.78539891644121695, 12.99999999999979927 ) ) ;
#4240 = AXIS2_PLACEMENT_3D ( 'NONE', #21065, #20945, #2790 ) ;
#4241 = DIRECTION ( 'NONE',  ( 0.005235963827102643048, -0.9999862922474495042, 7.723249237701186312E-15 ) ) ;
#4242 = ORIENTED_EDGE ( 'NONE', *, *, #12170, .T. ) ;
#4243 = COORDINATED_UNIVERSAL_TIME_OFFSET ( 0, 0, .AHEAD. ) ;
#4244 = CARTESIAN_POINT ( 'NONE',  ( 53.10252809683457542, 27.27557781334508036, 2.066999999999991733 ) ) ;
#4245 = ORIENTED_EDGE ( 'NONE', *, *, #13068, .T. ) ;
#4246 = VERTEX_POINT ( 'NONE', #4692 ) ;
#4247 = EDGE_CURVE ( 'NONE', #15424, #7095, #16030, .T. ) ;
#4248 = CALENDAR_DATE ( 2026, 31, 10 ) ;
#4249 = CARTESIAN_POINT ( 'NONE',  ( -62.74088165156670271, -25.10566213532069924, -5.538319619822460249E-15 ) ) ;
#4250 = EDGE_CURVE ( 'NONE', #5973, #6701, #8465, .T. ) ;
#4251 = ORIENTED_EDGE ( 'NONE', *, *, #5487, .F. ) ;
#4252 = EDGE_LOOP ( 'NONE', ( #17084, #10538, #21689, #10347 ) ) ;
#4253 = CARTESIAN_POINT ( 'NONE',  ( 31.37708959083939675, -0.2124270449898580104, -13.00000000000039968 ) ) ;
#4254 = PERSON_AND_ORGANIZATION ( #11966, #8758 ) ;
#4255 = LOCAL_TIME ( 14, 11, 27.00000000000000000, #21052 ) ;
#4256 = PERSON_AND_ORGANIZATION ( #1406, #20905 ) ;
#4257 = CARTESIAN_POINT ( 'NONE',  ( 80.84056339148629888, -0.9497634067828859550, 3.641582893490300021E-14 ) ) ;
#4258 = AXIS2_PLACEMENT_3D ( 'NONE', #18151, #5546, #426 ) ;
#4259 = PERSON ( 'NAUO-PER37', 'UNSPECIFIED', 'UNSPECIFIED', ('UNSPECIFIED'), ('UNSPECIFIED'), ('UNSPECIFIED') ) ;
#4260 = EDGE_CURVE ( 'NONE', #12862, #10685, #22957, .T. ) ;
#4261 = VECTOR ( 'NONE', #17550, 1000.000000000000114 ) ;
#4262 = EDGE_CURVE ( 'NONE', #2609, #10848, #12308, .T. ) ;
#4263 = CIRCLE ( 'NONE', #2359, 2.600000000000000089 ) ;
#4264 = VECTOR ( 'NONE', #3856, 1000.000000000000000 ) ;
#4265 =( NAMED_UNIT ( * ) PLANE_ANGLE_UNIT ( ) SI_UNIT ( $, .RADIAN. ) );
#4266 = CC_DESIGN_APPROVAL ( #921, ( #1214 ) ) ;
#4267 = CARTESIAN_POINT ( 'NONE',  ( 49.94654008041209892, 6.372928970669730298, 3.830789599272820115E-14 ) ) ;
#4268 = ORIENTED_EDGE ( 'NONE', *, *, #6357, .F. ) ;
#4269 = APPLICATION_CONTEXT ( 'configuration controlled 3d designs of mechanical parts and assemblies' ) ;
#4270 = CIRCLE ( 'NONE', #9201, 2.500000000000000444 ) ;
#4271 = DATE_AND_TIME ( #4027, #11788 ) ;
#4272 = ORIENTED_EDGE ( 'NONE', *, *, #15333, .T. ) ;
#4273 = AXIS2_PLACEMENT_3D ( 'NONE', #6781, #14006, #8911 ) ;
#4274 = LINE ( 'NONE', #18780, #22419 ) ;
#4275 = ORIENTED_EDGE ( 'NONE', *, *, #16837, .T. ) ;
#4276 = CC_DESIGN_APPROVAL ( #23437, ( #15652 ) ) ;
#4277 = CARTESIAN_POINT ( 'NONE',  ( 113.2956221386590130, -28.78551670568859677, -2.700000000000000178 ) ) ;
#4278 = DIRECTION ( 'NONE',  ( 0.2306359803922085339, 0.9730401042858022320, 0.000000000000000000 ) ) ;
#4279 = CARTESIAN_POINT ( 'NONE',  ( -20.00000000000000000, -20.00000000000000000, 5.000000000004559908 ) ) ;
#4280 = ORIENTED_EDGE ( 'NONE', *, *, #17496, .F. ) ;
#4281 = ORIENTED_EDGE ( 'NONE', *, *, #5923, .T. ) ;
#4282 = DIRECTION ( 'NONE',  ( -0.9730401042858035643, 0.2306359803922028717, 5.958148513035547083E-17 ) ) ;
#4283 = CIRCLE ( 'NONE', #3120, 0.0009999999996440807337 ) ;
#4284 = ORIENTED_EDGE ( 'NONE', *, *, #8922, .F. ) ;
#4285 = AXIS2_PLACEMENT_3D ( 'NONE', #18130, #21552, #12782 ) ;
#4286 = PERSON_AND_ORGANIZATION ( #11966, #8758 ) ;
#4287 = PERSON ( 'NAUO-PER10', 'UNSPECIFIED', 'UNSPECIFIED', ('UNSPECIFIED'), ('UNSPECIFIED'), ('UNSPECIFIED') ) ;
#4288 = EDGE_CURVE ( 'NONE', #21240, #238, #4662, .T. ) ;
#4289 = ORIENTED_EDGE ( 'NONE', *, *, #19831, .T. ) ;
#4290 = VECTOR ( 'NONE', #11233, 999.9999999999998863 ) ;
#4291 = EDGE_LOOP ( 'NONE', ( #13978, #8585 ) ) ;
#4292 = DIRECTION ( 'NONE',  ( 6.123237831918399306E-17, -1.569224110909209817E-30, -1.000000000000000000 ) ) ;
#4293 = CALENDAR_DATE ( 2026, 31, 10 ) ;
#4294 = FACE_OUTER_BOUND ( 'NONE', #11988, .T. ) ;
#4295 = APPROVAL ( #2596, 'UNKNOWN' ) ;
#4296 = CC_DESIGN_PERSON_AND_ORGANIZATION_ASSIGNMENT ( #22672, #22444, ( #14859 ) ) ;
#4297 = CARTESIAN_POINT ( 'NONE',  ( -27.50000000434249969, 26.95208919188020147, 6.750000000004539480 ) ) ;
#4298 = CIRCLE ( 'NONE', #4315, 4.750000000000000000 ) ;
#4299 = VECTOR ( 'NONE', #17712, 999.9999999999998863 ) ;
#4300 = EDGE_CURVE ( 'NONE', #20392, #12727, #12407, .T. ) ;
#4301 = EDGE_CURVE ( 'NONE', #6326, #15757, #19080, .T. ) ;
#4302 = SECURITY_CLASSIFICATION ( '', '', #10915 ) ;
#4303 = CIRCLE ( 'NONE', #23240, 2.499999999999998668 ) ;
#4304 = VECTOR ( 'NONE', #2057, 1000.000000000000114 ) ;
#4305 = DIRECTION ( 'NONE',  ( -1.187319687680494078E-16, -2.805478249478340539E-20, -1.000000000000000000 ) ) ;
#4306 = PERSON_AND_ORGANIZATION ( #11966, #8758 ) ;
#4307 = CIRCLE ( 'NONE', #14169, 2.067000000000000615 ) ;
#4308 = ORIENTED_EDGE ( 'NONE', *, *, #10796, .T. ) ;
#4309 = CARTESIAN_POINT ( 'NONE',  ( -69.83648240813081998, -6.865755409778439677, -0.01852613985921119921 ) ) ;
#4310 = DIRECTION ( 'NONE',  ( -0.2306359803922026497, -0.9730401042858035643, 0.000000000000000000 ) ) ;
#4311 = EDGE_LOOP ( 'NONE', ( #7847, #4004, #9289, #17638 ) ) ;
#4312 = CARTESIAN_POINT ( 'NONE',  ( 39.27359436029428963, 22.26288585089417538, -8.750000000000499156 ) ) ;
#4313 = DIRECTION ( 'NONE',  ( 1.000000000000000000, 3.210834492181040124E-17, 1.751623080406019734E-47 ) ) ;
#4314 = EDGE_LOOP ( 'NONE', ( #22219, #15549, #14909, #2501 ) ) ;
#4315 = AXIS2_PLACEMENT_3D ( 'NONE', #20247, #7537, #18713 ) ;
#4316 = CARTESIAN_POINT ( 'NONE',  ( 39.37089837072279863, 22.23982225285499936, -13.00000000000049916 ) ) ;
#4317 = APPLICATION_PROTOCOL_DEFINITION ( 'international standard', 'config_control_design', 1994, #5795 ) ;
#4318 = EDGE_CURVE ( 'NONE', #11510, #17116, #17281, .T. ) ;
#4319 = LOCAL_TIME ( 14, 11, 27.00000000000000000, #12873 ) ;
#4320 = VECTOR ( 'NONE', #4587, 999.9999999999998863 ) ;
#4321 = ORIENTED_EDGE ( 'NONE', *, *, #10833, .F. ) ;
#4322 = ORIENTED_EDGE ( 'NONE', *, *, #5625, .F. ) ;
#4323 = CARTESIAN_POINT ( 'NONE',  ( 31.49419854219519976, 9.774809681453278998, -25.00000000000000000 ) ) ;
#4324 = FACE_OUTER_BOUND ( 'NONE', #11323, .T. ) ;
#4325 =( REPRESENTATION_RELATIONSHIP ('NONE','NONE', #18121, #19781 ) REPRESENTATION_RELATIONSHIP_WITH_TRANSFORMATION ( #22059 )SHAPE_REPRESENTATION_RELATIONSHIP( ) );
#4326 = ORIENTED_EDGE ( 'NONE', *, *, #18959, .T. ) ;
#4327 = SHAPE_DEFINITION_REPRESENTATION ( #7029, #14436 ) ;
#4328 = DIRECTION ( 'NONE',  ( -1.187319687680494078E-16, -2.805478249478340539E-20, -1.000000000000000000 ) ) ;
#4329 = VECTOR ( 'NONE', #1263, 1000.000000000000000 ) ;
#4330 = CARTESIAN_POINT ( 'NONE',  ( -30.79248430819439974, 6.338858557519069237, 2.999000000000090260 ) ) ;
#4331 = PERSON_AND_ORGANIZATION_ROLE ( 'classification_officer' ) ;
#4332 = DIRECTION ( 'NONE',  ( -1.138590270679730064E-14, -2.220446049251235259E-15, -1.000000000000000000 ) ) ;
#4333 = ADVANCED_FACE ( 'NONE', ( #17990 ), #12646, .F. ) ;
#4334 = EDGE_CURVE ( 'NONE', #3009, #11143, #21340, .T. ) ;
#4335 = DIRECTION ( 'NONE',  ( 6.124378941434239724E-17, -2.274246353359159970E-33, 1.000000000000000000 ) ) ;
#4336 = FACE_OUTER_BOUND ( 'NONE', #12032, .T. ) ;
#4337 = APPROVAL_DATE_TIME ( #17022, #3940 ) ;
#4338 = CIRCLE ( 'NONE', #17612, 2.499999999999998668 ) ;
#4339 = DIRECTION ( 'NONE',  ( -0.2306359803922030105, -0.9730401042858034533, 0.000000000000000000 ) ) ;
#4340 = AXIS2_PLACEMENT_3D ( 'NONE', #19000, #15075, #1042 ) ;
#4341 = CARTESIAN_POINT ( 'NONE',  ( 113.2956221386590130, -28.78551670568859677, -2.700000000000000178 ) ) ;
#4342 = DIRECTION ( 'NONE',  ( -2.269747459788994803E-13, -2.220446049250320181E-15, -1.000000000000000000 ) ) ;
#4343 = DIRECTION ( 'NONE',  ( -0.2306359803922033436, -0.9730401042858034533, 0.000000000000000000 ) ) ;
#4344 = LINE ( 'NONE', #22140, #20966 ) ;
#4345 = ORIENTED_EDGE ( 'NONE', *, *, #20302, .F. ) ;
#4346 = ADVANCED_FACE ( 'NONE', ( #21984 ), #14755, .T. ) ;
#4347 = ORIENTED_EDGE ( 'NONE', *, *, #13493, .F. ) ;
#4348 = CARTESIAN_POINT ( 'NONE',  ( 41.24356139695900225, 11.92996613406550033, 15.90000000000000036 ) ) ;
#4349 = FACE_OUTER_BOUND ( 'NONE', #21255, .T. ) ;
#4350 = ORIENTED_EDGE ( 'NONE', *, *, #2727, .F. ) ;
#4351 = CARTESIAN_POINT ( 'NONE',  ( 6.500000000000000000, -17.30000000000000071, 2.500000000000000000 ) ) ;
#4352 = ORIENTED_EDGE ( 'NONE', *, *, #18811, .T. ) ;
#4353 = FACE_OUTER_BOUND ( 'NONE', #18791, .T. ) ;
#4354 = CALENDAR_DATE ( 2026, 31, 10 ) ;
#4355 = CARTESIAN_POINT ( 'NONE',  ( 37.63679421689584359, 9.430002510136448635, -9.000012045631684998 ) ) ;
#4356 = EDGE_CURVE ( 'NONE', #20891, #8556, #11123, .T. ) ;
#4357 = ADVANCED_FACE ( 'NONE', ( #18205, #1575 ), #3712, .T. ) ;
#4358 = CONTEXT_DEPENDENT_SHAPE_REPRESENTATION ( #11306, #16492 ) ;
#4359 = CARTESIAN_POINT ( 'NONE',  ( 3.499952022866073431, 0.01832587339492582415, 2.500000000000089706 ) ) ;
#4360 = DIRECTION ( 'NONE',  ( -1.734723475976802677E-14, -4.336808689942006376E-14, -1.000000000000000000 ) ) ;
#4361 = ORIENTED_EDGE ( 'NONE', *, *, #9591, .T. ) ;
#4362 = CARTESIAN_POINT ( 'NONE',  ( -3.499952022866071211, -0.01832587339492760051, -8.848002871973867878E-14 ) ) ;
#4363 = CARTESIAN_POINT ( 'NONE',  ( 27.91817548414393713, -6.133715391986834575, 13.00000000000019895 ) ) ;
#4364 = EDGE_LOOP ( 'NONE', ( #7729, #20577 ) ) ;
#4365 = CARTESIAN_POINT ( 'NONE',  ( -26.00000000397269773, 22.95208919201850151, 8.000000000004529710 ) ) ;
#4366 = PLANE ( 'NONE',  #6106 ) ;
#4367 = EDGE_LOOP ( 'NONE', ( #16638, #15678, #11628, #12234 ) ) ;
#4368 = VECTOR ( 'NONE', #17558, 1000.000000000000000 ) ;
#4369 = UNCERTAINTY_MEASURE_WITH_UNIT (LENGTH_MEASURE( 1.000000000000000082E-05 ), #17141, 'distance_accuracy_value', 'NONE');
#4370 = DATE_TIME_ROLE ( 'classification_date' ) ;
#4371 = CARTESIAN_POINT ( 'NONE',  ( -67.06978017061331343, -25.35162245663349978, 2.500000000000000000 ) ) ;
#4372 = ORIENTED_EDGE ( 'NONE', *, *, #4721, .T. ) ;
#4373 = CC_DESIGN_PERSON_AND_ORGANIZATION_ASSIGNMENT ( #15478, #10157, ( #9917 ) ) ;
#4374 = DATE_AND_TIME ( #5449, #16350 ) ;
#4375 = CARTESIAN_POINT ( 'NONE',  ( 36.76922337734900026, -6.947011889080330960, 20.00000000000000000 ) ) ;
#4376 = ORIENTED_EDGE ( 'NONE', *, *, #13043, .T. ) ;
#4377 = ORIENTED_EDGE ( 'NONE', *, *, #3021, .T. ) ;
#4378 = APPROVAL_ROLE ( '' ) ;
#4379 = AXIS2_PLACEMENT_3D ( 'NONE', #23057, #7372, #18050 ) ;
#4380 = COORDINATED_UNIVERSAL_TIME_OFFSET ( 0, 0, .AHEAD. ) ;
#4381 = CARTESIAN_POINT ( 'NONE',  ( 35.59419854219520118, 9.774809681453330512, -17.70000000000050022 ) ) ;
#4382 = DIRECTION ( 'NONE',  ( 2.982858504489129897E-17, -2.441916418604790135E-15, -1.000000000000000000 ) ) ;
#4383 = VERTEX_POINT ( 'NONE', #19884 ) ;
#4384 = EDGE_CURVE ( 'NONE', #3768, #4115, #12521, .T. ) ;
#4385 = APPROVAL_ROLE ( '' ) ;
#4386 = PRODUCT_DEFINITION_SHAPE ( 'NONE', 'NONE',  #5042 ) ;
#4387 = ORIENTED_EDGE ( 'NONE', *, *, #19285, .T. ) ;
#4388 = CARTESIAN_POINT ( 'NONE',  ( 37.48968750243700043, 22.68571848161329996, 13.00000000000000000 ) ) ;
#4389 = CARTESIAN_POINT ( 'NONE',  ( -30.72441677844230057, -6.660963241697680282, 3.000000000000090150 ) ) ;
#4390 = ORIENTED_EDGE ( 'NONE', *, *, #22885, .T. ) ;
#4391 = LINE ( 'NONE', #14719, #2189 ) ;
#4392 = AXIS2_PLACEMENT_3D ( 'NONE', #8895, #23463, #12794 ) ;
#4393 = DIRECTION ( 'NONE',  ( -0.9730401042858024541, 0.2306359803922080898, 5.959266323858942451E-17 ) ) ;
#4394 = CARTESIAN_POINT ( 'NONE',  ( -27.00000000000000000, -27.34999999999999787, 5.000000000000000000 ) ) ;
#4395 = EDGE_LOOP ( 'NONE', ( #8277, #51, #14788 ) ) ;
#4396 = VERTEX_POINT ( 'NONE', #10759 ) ;
#4397 = LINE ( 'NONE', #9867, #18192 ) ;
#4398 = ORIENTED_EDGE ( 'NONE', *, *, #6234, .F. ) ;
#4399 = PERSON_AND_ORGANIZATION_ROLE ( 'design_owner' ) ;
#4400 = AXIS2_PLACEMENT_3D ( 'NONE', #12927, #7370, #12708 ) ;
#4401 = VERTEX_POINT ( 'NONE', #3825 ) ;
#4402 = ORIENTED_EDGE ( 'NONE', *, *, #22820, .T. ) ;
#4403 = CARTESIAN_POINT ( 'NONE',  ( -19.49999999982360066, -0.1021026942259749964, -2.500000000000000000 ) ) ;
#4404 = PERSON_AND_ORGANIZATION_ROLE ( 'creator' ) ;
#4405 = DIRECTION ( 'NONE',  ( 0.000000000000000000, 0.000000000000000000, -1.000000000000000000 ) ) ;
#4406 = CARTESIAN_POINT ( 'NONE',  ( -58.51256015200321059, 7.693735815438545345, 2.108981951733699184E-15 ) ) ;
#4407 = DIRECTION ( 'NONE',  ( 0.000000000000000000, 0.000000000000000000, 1.000000000000000000 ) ) ;
#4408 = AXIS2_PLACEMENT_3D ( 'NONE', #4297, #6540, #8206 ) ;
#4409 = DIRECTION ( 'NONE',  ( -0.6944962871189666043, 0.7194962871189606313, 0.000000000000000000 ) ) ;
#4410 = EDGE_CURVE ( 'NONE', #11739, #14649, #8954, .T. ) ;
#4411 = APPROVAL_DATE_TIME ( #1183, #20903 ) ;
#4412 = ORIENTED_EDGE ( 'NONE', *, *, #23193, .F. ) ;
#4413 = LINE ( 'NONE', #2514, #14045 ) ;
#4414 = DIRECTION ( 'NONE',  ( -0.2306359803921919083, -0.9730401042858062288, -1.333568672157176260E-13 ) ) ;
#4415 = ORIENTED_EDGE ( 'NONE', *, *, #2567, .T. ) ;
#4416 = APPROVAL ( #14798, 'UNKNOWN' ) ;
#4417 = CARTESIAN_POINT ( 'NONE',  ( 44.35571774535060996, 23.18255965125822371, 13.00000000000000000 ) ) ;
#4418 = CARTESIAN_POINT ( 'NONE',  ( -20.00000001748994549, -17.37500000000000000, -8.249999999995464961 ) ) ;
#4419 = ORIENTED_EDGE ( 'NONE', *, *, #19847, .T. ) ;
#4420 = FACE_OUTER_BOUND ( 'NONE', #22781, .T. ) ;
#4421 = EDGE_CURVE ( 'NONE', #3781, #20776, #14611, .T. ) ;
#4422 = ADVANCED_FACE ( 'NONE', ( #16527 ), #253, .F. ) ;
#4423 = PERSON_AND_ORGANIZATION ( #11966, #8758 ) ;
#4424 = CONICAL_SURFACE ( 'NONE', #18865, 2.283500000000000529, 0.7853981633974476129 ) ;
#4425 = ORIENTED_EDGE ( 'NONE', *, *, #11909, .T. ) ;
#4426 = ORIENTED_EDGE ( 'NONE', *, *, #3595, .F. ) ;
#4427 = CARTESIAN_POINT ( 'NONE',  ( -20.00000000397270128, 22.95208919256889857, -4.999999999995559996 ) ) ;
#4428 = CIRCLE ( 'NONE', #12771, 2.369999999999999218 ) ;
#4429 = LINE ( 'NONE', #11699, #15906 ) ;
#4430 = ORIENTED_EDGE ( 'NONE', *, *, #10660, .F. ) ;
#4431 = DATE_AND_TIME ( #20697, #11073 ) ;
#4432 = CARTESIAN_POINT ( 'NONE',  ( 46.46175228317039796, -6.161274394849590053, 13.00000000000000000 ) ) ;
#4433 = CARTESIAN_POINT ( 'NONE',  ( 118.4388045014059969, -7.086722380115130449, 19.59999999999999787 ) ) ;
#4434 = SECURITY_CLASSIFICATION_LEVEL ( 'unclassified' ) ;
#4435 = CARTESIAN_POINT ( 'NONE',  ( 49.97703550743810297, 19.72589006657999988, -10.50000000000049916 ) ) ;
#4436 = CIRCLE ( 'NONE', #14670, 4.999999999999998224 ) ;
#4437 = CARTESIAN_POINT ( 'NONE',  ( -20.00000000397459843, 22.95208919257349933, -7.999999999995569766 ) ) ;
#4438 = EDGE_CURVE ( 'NONE', #12469, #15535, #19815, .T. ) ;
#4439 = APPROVAL_STATUS ( 'not_yet_approved' ) ;
#4440 = CIRCLE ( 'NONE', #2915, 6.500000000000000888 ) ;
#4441 = VECTOR ( 'NONE', #10978, 1000.000000000000227 ) ;
#4442 = DIRECTION ( 'NONE',  ( -1.187319687680494078E-16, -2.805478249478275539E-20, -1.000000000000000000 ) ) ;
#4443 = DIRECTION ( 'NONE',  ( -0.2306359803922033713, -0.9730401042858033422, 5.180237729619581644E-15 ) ) ;
#4444 = PRODUCT_RELATED_PRODUCT_CATEGORY ( 'detail', '', ( #18416 ) ) ;
#4445 = FACE_OUTER_BOUND ( 'NONE', #23098, .T. ) ;
#4446 = CARTESIAN_POINT ( 'NONE',  ( -0.5391976746782192187, 18.33937061236849075, 4.999999999999997335 ) ) ;
#4447 = CC_DESIGN_PERSON_AND_ORGANIZATION_ASSIGNMENT ( #1669, #19856, ( #15730 ) ) ;
#4448 = CIRCLE ( 'NONE', #19248, 0.0009999999999225038516 ) ;
#4449 = DIRECTION ( 'NONE',  ( 3.210834492194360164E-17, -2.441916418604790135E-15, -1.000000000000000000 ) ) ;
#4450 = ADVANCED_FACE ( 'NONE', ( #20687 ), #11872, .F. ) ;
#4452 = ORIENTED_EDGE ( 'NONE', *, *, #13697, .T. ) ;
#4451 = ADVANCED_FACE ( 'NONE', ( #2412, #2164, #13457, #4420, #6214, #22573 ), #497, .F. ) ;
#4453 = CC_DESIGN_PERSON_AND_ORGANIZATION_ASSIGNMENT ( #9784, #17006, ( #3606 ) ) ;
#4454 = ORIENTED_EDGE ( 'NONE', *, *, #2235, .T. ) ;
#4455 = CARTESIAN_POINT ( 'NONE',  ( -17.47493719149800029, 26.45208920939580111, -5.499999999996139977 ) ) ;
#4456 = SHAPE_REPRESENTATION ( 'Pin00', ( #12739 ), #10268 ) ;
#4457 = DIRECTION ( 'NONE',  ( 5.798605125234323991E-17, -1.374421231021384554E-17, 1.000000000000000000 ) ) ;
#4458 = CIRCLE ( 'NONE', #20370, 2.499999999999998668 ) ;
#4459 = ORIENTED_EDGE ( 'NONE', *, *, #5727, .F. ) ;
#4460 = CYLINDRICAL_SURFACE ( 'NONE', #7686, 2.500000000000000000 ) ;
#4461 = CIRCLE ( 'NONE', #17738, 4.999999999999995559 ) ;
#4462 = ORIENTED_EDGE ( 'NONE', *, *, #14588, .F. ) ;
#4463 = DIRECTION ( 'NONE',  ( 0.9730401042858024541, -0.2306359803922080898, -5.959266323854002210E-17 ) ) ;
#4464 = CIRCLE ( 'NONE', #17742, 2.499999999999999112 ) ;
#4465 = APPROVAL_STATUS ( 'not_yet_approved' ) ;
#4466 = DIRECTION ( 'NONE',  ( 0.9730401042858024541, -0.2306359803922080898, -5.959266323858942451E-17 ) ) ;
#4467 = DATE_TIME_ROLE ( 'classification_date' ) ;
#4468 = CARTESIAN_POINT ( 'NONE',  ( 43.81897180516431689, 0.03336243584794939404, -25.00000000000000000 ) ) ;
#4469 = EDGE_CURVE ( 'NONE', #2592, #23382, #4270, .T. ) ;
#4470 = AXIS2_PLACEMENT_3D ( 'NONE', #17828, #16496, #14255 ) ;
#4471 = LINE ( 'NONE', #546, #20623 ) ;
#4472 = VERTEX_POINT ( 'NONE', #11582 ) ;
#4473 = DIRECTION ( 'NONE',  ( -0.2306359803922041485, -0.9730401042858032312, 4.373252460445728664E-15 ) ) ;
#4474 = VECTOR ( 'NONE', #632, 1000.000000000000000 ) ;
#4475 = ADVANCED_FACE ( 'NONE', ( #18917 ), #18693, .F. ) ;
#4476 = CARTESIAN_POINT ( 'NONE',  ( 37.27955344062029752, 9.375336445360778370, 27.68999999999999773 ) ) ;
#4477 = EDGE_LOOP ( 'NONE', ( #17805, #5906, #642, #11314 ) ) ;
#4478 = CARTESIAN_POINT ( 'NONE',  ( -0.7498608572560920837, 18.38930330212339825, -2.632567431446439807E-17 ) ) ;
#4479 = CARTESIAN_POINT ( 'NONE',  ( -0.5391976746803449627, 18.33937061236850141, -7.621247264287879719E-15 ) ) ;
#4480 = EDGE_CURVE ( 'NONE', #18764, #2592, #17919, .T. ) ;
#4481 = DATE_AND_TIME ( #11863, #9924 ) ;
#4482 = EDGE_CURVE ( 'NONE', #15538, #1008, #9896, .T. ) ;
#4483 = CARTESIAN_POINT ( 'NONE',  ( 29.76326332728156032, 1.650605442299594827, 13.00000000000019895 ) ) ;
#4484 = ORIENTED_EDGE ( 'NONE', *, *, #13660, .T. ) ;
#4485 = DATE_AND_TIME ( #10323, #6510 ) ;
#4486 = DIRECTION ( 'NONE',  ( 0.2306359803922032325, 0.9730401042858035643, -1.407521210652540462E-17 ) ) ;
#4487 = ORIENTED_EDGE ( 'NONE', *, *, #12235, .T. ) ;
#4488 = ORIENTED_EDGE ( 'NONE', *, *, #7740, .T. ) ;
#4489 = VECTOR ( 'NONE', #8553, 1000.000000000000000 ) ;
#4490 = PERSON_AND_ORGANIZATION_ROLE ( 'classification_officer' ) ;
#4491 = PERSON_AND_ORGANIZATION_ROLE ( 'classification_officer' ) ;
#4492 = AXIS2_PLACEMENT_3D ( 'NONE', #6942, #5141, #5369 ) ;
#4493 = CARTESIAN_POINT ( 'NONE',  ( -69.91240388362392366, 7.634045827809356588, -7.200000000000000178 ) ) ;
#4494 = FACE_BOUND ( 'NONE', #10057, .T. ) ;
#4495 = ORIENTED_EDGE ( 'NONE', *, *, #2097, .F. ) ;
#4496 = PERSON_AND_ORGANIZATION ( #11966, #8758 ) ;
#4497 = ORIENTED_EDGE ( 'NONE', *, *, #20411, .T. ) ;
#4498 = DIRECTION ( 'NONE',  ( 0.9730401042858035643, -0.2306359803922028717, -5.959266323858677443E-17 ) ) ;
#4499 = DIRECTION ( 'NONE',  ( 0.000000000000000000, 0.000000000000000000, 1.000000000000000000 ) ) ;
#4500 = ORIENTED_EDGE ( 'NONE', *, *, #817, .F. ) ;
#4501 = CARTESIAN_POINT ( 'NONE',  ( -14.00000000397270128, 22.95208919312850071, 5.500000000004400036 ) ) ;
#4502 = CLOSED_SHELL ( 'NONE', ( #8642, #6172, #17626, #18838 ) ) ;
#4504 = CIRCLE ( 'NONE', #9829, 4.250000000000000000 ) ;
#4503 = FACE_OUTER_BOUND ( 'NONE', #22318, .T. ) ;
#4505 = FACE_OUTER_BOUND ( 'NONE', #13681, .T. ) ;
#4506 = VERTEX_POINT ( 'NONE', #22466 ) ;
#4507 = ORIENTED_EDGE ( 'NONE', *, *, #449, .T. ) ;
#4508 = FACE_BOUND ( 'NONE', #4799, .T. ) ;
#4509 = ORIENTED_EDGE ( 'NONE', *, *, #18798, .T. ) ;
#4510 = APPROVAL_ROLE ( '' ) ;
#4511 = ORIENTED_EDGE ( 'NONE', *, *, #4687, .F. ) ;
#4512 = ORIENTED_EDGE ( 'NONE', *, *, #23140, .T. ) ;
#4513 = DIRECTION ( 'NONE',  ( -6.123230174520380038E-17, -4.962644601432260272E-15, -1.000000000000000000 ) ) ;
#4514 = SHAPE_DEFINITION_REPRESENTATION ( #18207, #13540 ) ;
#4515 = VECTOR ( 'NONE', #1229, 1000.000000000000000 ) ;
#4516 = EDGE_CURVE ( 'NONE', #7758, #7718, #17125, .T. ) ;
#4517 = CYLINDRICAL_SURFACE ( 'NONE', #4408, 2.500000000000002220 ) ;
#4518 = DIRECTION ( 'NONE',  ( 1.000000000000000000, 0.000000000000000000, 0.000000000000000000 ) ) ;
#4519 = CC_DESIGN_PERSON_AND_ORGANIZATION_ASSIGNMENT ( #8972, #1472, ( #3013 ) ) ;
#4520 = CARTESIAN_POINT ( 'NONE',  ( -60.04781580374580585, 11.89276268270289982, -5.000000000000000000 ) ) ;
#4521 = SECURITY_CLASSIFICATION_LEVEL ( 'unclassified' ) ;
#4522 = EDGE_LOOP ( 'NONE', ( #16197, #13682, #20196, #637 ) ) ;
#4523 = ORGANIZATION ( 'NAUO-ORG8', 'UNSPECIFIED', 'UNSPECIFIED' ) ;
#4524 = CARTESIAN_POINT ( 'NONE',  ( 30.57814311865390167, -3.583136841839989817, 11.00000000000019895 ) ) ;
#4525 = VECTOR ( 'NONE', #12651, 1000.000000000000000 ) ;
#4526 = DIRECTION ( 'NONE',  ( 0.000000000000000000, 0.000000000000000000, -1.000000000000000000 ) ) ;
#4527 = ORIENTED_EDGE ( 'NONE', *, *, #19511, .F. ) ;
#4528 = DIRECTION ( 'NONE',  ( 0.000000000000000000, 4.336808689942006376E-14, 1.000000000000000000 ) ) ;
#4529 = CARTESIAN_POINT ( 'NONE',  ( 30.89467803343007901, -3.022216679644092796, -11.00000000000039257 ) ) ;
#4530 = ORIENTED_EDGE ( 'NONE', *, *, #6919, .T. ) ;
#4531 = DIRECTION ( 'NONE',  ( -0.2306359803922076457, -0.9730401042858025651, 0.000000000000000000 ) ) ;
#4532 = CALENDAR_DATE ( 2026, 31, 10 ) ;
#4533 = ORIENTED_EDGE ( 'NONE', *, *, #19898, .T. ) ;
#4534 = ORIENTED_EDGE ( 'NONE', *, *, #15298, .T. ) ;
#4535 = CARTESIAN_POINT ( 'NONE',  ( -20.00000000000000000, -20.00000000000000000, 5.000000000004559908 ) ) ;
#4536 = CARTESIAN_POINT ( 'NONE',  ( -20.00000001832276553, -17.25000000000000000, -8.499999999995466737 ) ) ;
#4537 = VERTEX_POINT ( 'NONE', #2522 ) ;
#4538 = DATE_TIME_ROLE ( 'creation_date' ) ;
#4539 = ADVANCED_FACE ( 'NONE', ( #18570 ), #8118, .F. ) ;
#4540 = LINE ( 'NONE', #18925, #15299 ) ;
#4541 = ADVANCED_FACE ( 'NONE', ( #9423 ), #9542, .F. ) ;
#4542 = DIRECTION ( 'NONE',  ( -0.005235963827102643048, 0.9999862922474495042, 7.724582913192744961E-15 ) ) ;
#4543 = CIRCLE ( 'NONE', #20848, 5.000000000000001776 ) ;
#4544 = AXIS2_PLACEMENT_3D ( 'NONE', #5025, #8595, #1685 ) ;
#4545 = DATE_TIME_ROLE ( 'classification_date' ) ;
#4546 = AXIS2_PLACEMENT_3D ( 'NONE', #13889, #2961, #6776 ) ;
#4547 = FACE_OUTER_BOUND ( 'NONE', #21661, .T. ) ;
#4548 = PERSON ( 'NAUO-PER34', 'UNSPECIFIED', 'UNSPECIFIED', ('UNSPECIFIED'), ('UNSPECIFIED'), ('UNSPECIFIED') ) ;
#4549 = EDGE_CURVE ( 'NONE', #8090, #2844, #9783, .T. ) ;
#4550 = ADVANCED_FACE ( 'NONE', ( #5856 ), #16886, .T. ) ;
#4551 = CARTESIAN_POINT ( 'NONE',  ( -17.47493719149830227, 26.45208920939580111, -6.749999999996139977 ) ) ;
#4552 = PERSON_AND_ORGANIZATION ( #11966, #8758 ) ;
#4553 = DIRECTION ( 'NONE',  ( -5.964507377817318600E-17, -4.861311874385510251E-15, -1.000000000000000000 ) ) ;
#4554 = DIRECTION ( 'NONE',  ( -0.2306359803922084506, -0.9730401042858020100, 5.112869192352694760E-15 ) ) ;
#4555 = DIRECTION ( 'NONE',  ( -0.9730401042858035643, 0.2306359803922028717, 5.959266323858677443E-17 ) ) ;
#4556 = CC_DESIGN_APPROVAL ( #22432, ( #19033 ) ) ;
#4557 = CARTESIAN_POINT ( 'NONE',  ( 58.49563186522070168, 17.70675969991879839, -10.74538000000049820 ) ) ;
#4558 = CARTESIAN_POINT ( 'NONE',  ( -62.74088165156670271, -25.10566213532069924, -5.538319619822460249E-15 ) ) ;
#4559 = CARTESIAN_POINT ( 'NONE',  ( -21.99941224366415682, -0.1563100308134279803, -3.750000000000000000 ) ) ;
#4560 = VECTOR ( 'NONE', #170, 1000.000000000000227 ) ;
#4561 = VERTEX_POINT ( 'NONE', #7992 ) ;
#4562 = VERTEX_POINT ( 'NONE', #15226 ) ;
#4563 = LINE ( 'NONE', #17286, #21332 ) ;
#4564 = FACE_OUTER_BOUND ( 'NONE', #16918, .T. ) ;
#4565 = EDGE_LOOP ( 'NONE', ( #9397, #22070, #6321, #18081, #1021, #15861, #16933, #18625 ) ) ;
#4566 = VECTOR ( 'NONE', #17983, 1000.000000000000000 ) ;
#4567 = DIRECTION ( 'NONE',  ( -0.9997651245102238127, -0.02167246670447303680, 0.000000000000000000 ) ) ;
#4568 = ADVANCED_FACE ( 'NONE', ( #22220 ), #5965, .T. ) ;
#4569 = ORIENTED_EDGE ( 'NONE', *, *, #10985, .F. ) ;
#4570 = DIRECTION ( 'NONE',  ( -0.9730401042858035643, 0.2306359803922028717, 5.432877459303547053E-17 ) ) ;
#4571 = AXIS2_PLACEMENT_3D ( 'NONE', #21164, #13929, #3593 ) ;
#4572 = DATE_AND_TIME ( #4930, #5043 ) ;
#4573 = DIRECTION ( 'NONE',  ( -0.9730401042858022320, 0.2306359803922080343, 5.959266323858941219E-17 ) ) ;
#4574 = APPLICATION_CONTEXT ( 'configuration controlled 3d designs of mechanical parts and assemblies' ) ;
#4575 = CC_DESIGN_PERSON_AND_ORGANIZATION_ASSIGNMENT ( #7213, #14447, ( #14124 ) ) ;
#4576 = PRODUCT ( 'F3', 'F3', '', ( #11149 ) ) ;
#4577 = LOCAL_TIME ( 14, 11, 27.00000000000000000, #6082 ) ;
#4578 = PRODUCT_DEFINITION ( 'UNKNOWN', '', #7624, #8741 ) ;
#4579 = SECURITY_CLASSIFICATION_LEVEL ( 'unclassified' ) ;
#4580 = APPROVAL_PERSON_ORGANIZATION ( #13720, #15763, #11730 ) ;
#4581 = LINE ( 'NONE', #19539, #10384 ) ;
#4582 = ADVANCED_FACE ( 'NONE', ( #22337 ), #13336, .F. ) ;
#4583 = ADVANCED_FACE ( 'NONE', ( #21264, #1432 ), #4661, .T. ) ;
#4584 = DIRECTION ( 'NONE',  ( -1.426882515614939919E-15, -5.761552236122200693E-15, -1.000000000000000000 ) ) ;
#4585 = EDGE_CURVE ( 'NONE', #7299, #18104, #11101, .T. ) ;
#4586 = ADVANCED_FACE ( 'NONE', ( #17722 ), #19035, .T. ) ;
#4587 = DIRECTION ( 'NONE',  ( -0.9730401042858036753, 0.2306359803922028995, -2.804983810440358801E-16 ) ) ;
#4588 = ORIENTED_EDGE ( 'NONE', *, *, #19798, .T. ) ;
#4590 = CIRCLE ( 'NONE', #17866, 7.000000000000000888 ) ;
#4589 = CARTESIAN_POINT ( 'NONE',  ( 35.75979881747896627, 26.94964815373096556, 13.00000000000000000 ) ) ;
#4591 = DIRECTION ( 'NONE',  ( 6.123230199561459225E-17, 4.868008300101910084E-15, 1.000000000000000000 ) ) ;
#4592 = VERTEX_POINT ( 'NONE', #6685 ) ;
#4593 =( BOUNDED_CURVE ( )  B_SPLINE_CURVE ( 2, ( #9269, #9752, #20191 ),
 .UNSPECIFIED., .F., .F. ) 
 B_SPLINE_CURVE_WITH_KNOTS ( ( 3, 3 ),
 ( 0.000000000000000000, 0.5842180690389568998 ),
 .UNSPECIFIED. ) 
 CURVE ( )  GEOMETRIC_REPRESENTATION_ITEM ( )  RATIONAL_B_SPLINE_CURVE ( ( 1.000000000000000000, 1.154700538379249908, 1.000000000000000000 ) ) 
 REPRESENTATION_ITEM ( '' )  );
#4594 = CARTESIAN_POINT ( 'NONE',  ( 118.5310588935630136, -6.697506338400830650, -19.59999999999999787 ) ) ;
#4595 = DIRECTION ( 'NONE',  ( 0.2306359803922031215, 0.9730401042858033422, -1.407521210652540462E-17 ) ) ;
#4596 = APPROVAL_PERSON_ORGANIZATION ( #18546, #10430, #22083 ) ;
#4597 = PERSON_AND_ORGANIZATION ( #6537, #16721 ) ;
#4598 = CARTESIAN_POINT ( 'NONE',  ( 62.70840910389689782, 3.348031886875269869, 1.061114750357439988E-14 ) ) ;
#4599 = SECURITY_CLASSIFICATION ( '', '', #9772 ) ;
#4600 = VERTEX_POINT ( 'NONE', #8695 ) ;
#4601 = VERTEX_POINT ( 'NONE', #15925 ) ;
#4602 = APPROVAL_STATUS ( 'not_yet_approved' ) ;
#4603 = CARTESIAN_POINT ( 'NONE',  ( -31.64153798721130428, 6.334539654120280083, 2.500000000000000000 ) ) ;
#4604 = EDGE_CURVE ( 'NONE', #227, #19697, #3872, .T. ) ;
#4605 = ORIENTED_EDGE ( 'NONE', *, *, #16927, .T. ) ;
#4606 = DIRECTION ( 'NONE',  ( -0.6944962871189167553, 0.7194962871190087039, 0.000000000000000000 ) ) ;
#4607 = CARTESIAN_POINT ( 'NONE',  ( -8.080225385240009217, -15.72171916155420313, 5.000000000000000000 ) ) ;
#4608 = LOCAL_TIME ( 14, 11, 27.00000000000000000, #8894 ) ;
#4609 = APPROVAL_ROLE ( '' ) ;
#4610 = APPROVAL_ROLE ( '' ) ;
#4611 = FACE_OUTER_BOUND ( 'NONE', #23393, .T. ) ;
#4612 = EDGE_CURVE ( 'NONE', #15424, #15538, #15813, .T. ) ;
#4613 = EDGE_CURVE ( 'NONE', #15338, #18898, #19499, .T. ) ;
#4614 = CC_DESIGN_APPROVAL ( #3134, ( #16369 ) ) ;
#4615 = DIRECTION ( 'NONE',  ( 2.899533054064307511E-31, 4.861311874385510251E-15, 1.000000000000000000 ) ) ;
#4616 = AXIS2_PLACEMENT_3D ( 'NONE', #15186, #6651, #2607 ) ;
#4617 = ORIENTED_EDGE ( 'NONE', *, *, #10219, .T. ) ;
#4618 = VECTOR ( 'NONE', #15931, 1000.000000000000000 ) ;
#4619 = COORDINATED_UNIVERSAL_TIME_OFFSET ( 0, 0, .AHEAD. ) ;
#4620 = EDGE_LOOP ( 'NONE', ( #3414, #17551, #14019, #1046 ) ) ;
#4621 = ORGANIZATION ( 'NAUO-ORG24', 'UNSPECIFIED', 'UNSPECIFIED' ) ;
#4622 = DIRECTION ( 'NONE',  ( 0.000000000000000000, 0.000000000000000000, -1.000000000000000000 ) ) ;
#4623 = DIRECTION ( 'NONE',  ( -0.9730401042858024541, 0.2306359803922080898, 5.959266323858942451E-17 ) ) ;
#4624 = ORIENTED_EDGE ( 'NONE', *, *, #21314, .T. ) ;
#4625 = DIRECTION ( 'NONE',  ( 0.000000000000000000, -1.000000000000000000, 2.081668171172168119E-15 ) ) ;
#4626 = CARTESIAN_POINT ( 'NONE',  ( 35.79393516024158117, 10.61748713066611494, 27.18999999999999417 ) ) ;
#4627 = CYLINDRICAL_SURFACE ( 'NONE', #12653, 2.500000000000000000 ) ;
#4628 = ORIENTED_EDGE ( 'NONE', *, *, #22895, .T. ) ;
#4629 = EDGE_LOOP ( 'NONE', ( #9506, #15582, #12496, #15235 ) ) ;
#4630 = DIRECTION ( 'NONE',  ( -0.002617981913558544045, 0.4999931461237241970, -0.8660254037844389297 ) ) ;
#4631 = ORIENTED_EDGE ( 'NONE', *, *, #9826, .T. ) ;
#4632 = PERSON_AND_ORGANIZATION_ROLE ( 'design_owner' ) ;
#4633 = EDGE_CURVE ( 'NONE', #21933, #21767, #17475, .T. ) ;
#4634 = LOCAL_TIME ( 14, 11, 27.00000000000000000, #7160 ) ;
#4635 = VERTEX_POINT ( 'NONE', #10030 ) ;
#4636 = ORIENTED_EDGE ( 'NONE', *, *, #6302, .T. ) ;
#4637 = FACE_OUTER_BOUND ( 'NONE', #10933, .T. ) ;
#4638 = APPROVAL_DATE_TIME ( #7021, #12859 ) ;
#4639 = FACE_OUTER_BOUND ( 'NONE', #22424, .T. ) ;
#4640 = AXIS2_PLACEMENT_3D ( 'NONE', #15867, #10544, #10659 ) ;
#4641 = LOCAL_TIME ( 14, 11, 27.00000000000000000, #14589 ) ;
#4642 = ADVANCED_FACE ( 'NONE', ( #19157 ), #17370, .F. ) ;
#4643 = AXIS2_PLACEMENT_3D ( 'NONE', #12040, #1072, #22810 ) ;
#4644 = ADVANCED_FACE ( 'NONE', ( #6916 ), #19376, .F. ) ;
#4645 = CONICAL_SURFACE ( 'NONE', #17920, 5.386751345948120218, 1.047197551196598297 ) ;
#4646 =( LENGTH_UNIT ( ) NAMED_UNIT ( * ) SI_UNIT ( .MILLI., .METRE. ) );
#4647 = LINE ( 'NONE', #1060, #1062 ) ;
#4648 = DATE_TIME_ROLE ( 'creation_date' ) ;
#4649 = LOCAL_TIME ( 14, 11, 27.00000000000000000, #14242 ) ;
#4650 = ORIENTED_EDGE ( 'NONE', *, *, #8255, .F. ) ;
#4651 = CARTESIAN_POINT ( 'NONE',  ( 112.2904587062726876, 7.080247408215343263, 13.00000000000000000 ) ) ;
#4652 = VECTOR ( 'NONE', #20572, 1000.000000000000227 ) ;
#4653 = CARTESIAN_POINT ( 'NONE',  ( 35.59419854219520118, 9.774809681453278998, -26.50000000000049738 ) ) ;
#4654 = ORIENTED_EDGE ( 'NONE', *, *, #12971, .F. ) ;
#4655 = CIRCLE ( 'NONE', #7685, 2.500000000000000444 ) ;
#4656 = DIRECTION ( 'NONE',  ( -0.9730401042858035643, 0.2306359803922028717, -2.804983810440358308E-16 ) ) ;
#4657 = CIRCLE ( 'NONE', #10373, 2.500000000000001332 ) ;
#4658 = CARTESIAN_POINT ( 'NONE',  ( 30.84445860938240003, -2.459566909556700320, -13.00000000000039968 ) ) ;
#4659 = LINE ( 'NONE', #2760, #7303 ) ;
#4660 = EDGE_LOOP ( 'NONE', ( #18032, #19608, #16229, #4387 ) ) ;
#4661 = PLANE ( 'NONE',  #6544 ) ;
#4662 = CIRCLE ( 'NONE', #17940, 7.599342076785325695 ) ;
#4663 = CALENDAR_DATE ( 2026, 31, 10 ) ;
#4664 = ORIENTED_EDGE ( 'NONE', *, *, #10718, .F. ) ;
#4665 = ORIENTED_EDGE ( 'NONE', *, *, #17709, .T. ) ;
#4666 = LINE ( 'NONE', #6571, #12290 ) ;
#4667 = DIRECTION ( 'NONE',  ( -1.187319687680499994E-16, -2.805478249478560216E-20, -1.000000000000000000 ) ) ;
#4668 = VECTOR ( 'NONE', #15795, 1000.000000000000227 ) ;
#4669 = ORIENTED_EDGE ( 'NONE', *, *, #21173, .T. ) ;
#4670 = APPROVAL_DATE_TIME ( #11468, #778 ) ;
#4671 = AXIS2_PLACEMENT_3D ( 'NONE', #8182, #22418, #15408 ) ;
#4672 = CC_DESIGN_PERSON_AND_ORGANIZATION_ASSIGNMENT ( #3597, #1796, ( #14461 ) ) ;
#4673 = CARTESIAN_POINT ( 'NONE',  ( -62.73971250800079957, -25.32895006819559924, -5.260896414089139989E-15 ) ) ;
#4674 = CC_DESIGN_APPROVAL ( #15763, ( #9377 ) ) ;
#4675 = EDGE_CURVE ( 'NONE', #14157, #16389, #16768, .T. ) ;
#4676 = LINE ( 'NONE', #12052, #14681 ) ;
#4677 = PERSON_AND_ORGANIZATION_ROLE ( 'classification_officer' ) ;
#4678 = CIRCLE ( 'NONE', #5811, 2.500000000000000444 ) ;
#4679 = CARTESIAN_POINT ( 'NONE',  ( 52.05497947389309843, 22.85602965967900246, 2.067000000000033921 ) ) ;
#4680 = AXIS2_PLACEMENT_3D ( 'NONE', #9067, #14759, #12985 ) ;
#4681 = VECTOR ( 'NONE', #17488, 1000.000000000000114 ) ;
#4682 = CARTESIAN_POINT ( 'NONE',  ( -23.50000000000000000, -20.00000000000000000, -2.500000000000000000 ) ) ;
#4683 = APPROVAL_ROLE ( '' ) ;
#4684 = CARTESIAN_POINT ( 'NONE',  ( 33.97401642954523737, -0.5293161874332097394, 13.00000000000019895 ) ) ;
#4685 = CARTESIAN_POINT ( 'NONE',  ( 42.88107685774368605, 18.83855087449469679, -13.00000000000000000 ) ) ;
#4686 = DIRECTION ( 'NONE',  ( 1.000000000000000000, -6.124317834331790129E-17, 0.000000000000000000 ) ) ;
#4687 = EDGE_CURVE ( 'NONE', #23033, #4801, #8337, .T. ) ;
#4688 = CC_DESIGN_APPROVAL ( #6447, ( #5821 ) ) ;
#4689 = DIRECTION ( 'NONE',  ( -0.2306359803922080343, -0.9730401042858022320, -5.907067092757291018E-15 ) ) ;
#4690 = CARTESIAN_POINT ( 'NONE',  ( 37.27955344062029752, 9.375336445360510140, -29.25000000000050093 ) ) ;
#4691 = VECTOR ( 'NONE', #19817, 1000.000000000000227 ) ;
#4692 = CARTESIAN_POINT ( 'NONE',  ( 2.499999999999970246, -31.09999999999999787, 21.50000000000000000 ) ) ;
#4693 = ORIENTED_EDGE ( 'NONE', *, *, #13482, .T. ) ;
#4694 = AXIS2_PLACEMENT_3D ( 'NONE', #8883, #19320, #4718 ) ;
#4695 = ORIENTED_EDGE ( 'NONE', *, *, #16882, .F. ) ;
#4696 = CARTESIAN_POINT ( 'NONE',  ( 117.0319250210129951, -13.02226701625849969, -18.89999999999999858 ) ) ;
#4697 = DIRECTION ( 'NONE',  ( 6.124378941434239724E-17, -2.274246353359159970E-33, 1.000000000000000000 ) ) ;
#4698 = ORIENTED_EDGE ( 'NONE', *, *, #2727, .T. ) ;
#4699 = CARTESIAN_POINT ( 'NONE',  ( 113.4570673249340018, -28.10438863268850085, -2.700000000000000178 ) ) ;
#4700 = ORIENTED_EDGE ( 'NONE', *, *, #3849, .F. ) ;
#4701 = CARTESIAN_POINT ( 'NONE',  ( 2.169175203825789655, 15.45758013577720114, 4.500000000000000000 ) ) ;
#4702 = APPROVAL_DATE_TIME ( #17647, #15763 ) ;
#4703 = COORDINATED_UNIVERSAL_TIME_OFFSET ( 0, 0, .AHEAD. ) ;
#4704 = AXIS2_PLACEMENT_3D ( 'NONE', #2611, #20772, #20888 ) ;
#4705 = DIRECTION ( 'NONE',  ( -0.2306359803922090335, -0.9730401042858022320, 4.744007713284279563E-15 ) ) ;
#4706 = CARTESIAN_POINT ( 'NONE',  ( -26.99999999999961631, -1.360632482642508324E-14, -21.50000000000000000 ) ) ;
#4707 = CARTESIAN_POINT ( 'NONE',  ( 0.000000000000000000, 0.000000000000000000, 0.000000000000000000 ) ) ;
#4708 = CARTESIAN_POINT ( 'NONE',  ( 102.8131131701580046, 7.202356331284519797, 13.00000000000000000 ) ) ;
#4709 = ORIENTED_EDGE ( 'NONE', *, *, #21465, .T. ) ;
#4710 = CARTESIAN_POINT ( 'NONE',  ( 31.49315201223960159, -2.613324229818170252, -13.00000000000039968 ) ) ;
#4711 = EDGE_CURVE ( 'NONE', #19959, #12698, #11803, .T. ) ;
#4712 = DESIGN_CONTEXT ( 'detailed design', #9897, 'design' ) ;
#4713 = DIRECTION ( 'NONE',  ( 0.000000000000000000, 0.000000000000000000, -1.000000000000000000 ) ) ;
#4714 = ORIENTED_EDGE ( 'NONE', *, *, #3193, .F. ) ;
#4715 = CARTESIAN_POINT ( 'NONE',  ( -21.99941281109913760, -0.1562838609880462526, 3.750000000000000000 ) ) ;
#4716 = DIRECTION ( 'NONE',  ( 0.2306359803922030938, 0.9730401042858035643, -4.741332172907964454E-18 ) ) ;
#4717 = APPROVAL ( #1277, 'UNKNOWN' ) ;
#4718 = DIRECTION ( 'NONE',  ( 0.000000000000000000, -4.336808689942006376E-14, -1.000000000000000000 ) ) ;
#4719 = ORIENTED_EDGE ( 'NONE', *, *, #5990, .T. ) ;
#4720 = ORIENTED_EDGE ( 'NONE', *, *, #10277, .T. ) ;
#4721 = EDGE_CURVE ( 'NONE', #2989, #1142, #21043, .T. ) ;
#4722 = EDGE_CURVE ( 'NONE', #21863, #16294, #6165, .T. ) ;
#4723 = APPLICATION_PROTOCOL_DEFINITION ( 'international standard', 'config_control_design', 1994, #19592 ) ;
#4724 = DIRECTION ( 'NONE',  ( -0.2306359803922077290, -0.9730401042858024541, 0.000000000000000000 ) ) ;
#4725 = ORIENTED_EDGE ( 'NONE', *, *, #8798, .F. ) ;
#4726 = FACE_BOUND ( 'NONE', #5698, .T. ) ;
#4727 = APPROVAL_DATE_TIME ( #23103, #17381 ) ;
#4728 = PRODUCT ( '1602p_c_15', '1602p_c_15', '', ( #14510 ) ) ;
#4729 = CONTEXT_DEPENDENT_SHAPE_REPRESENTATION ( #18116, #7590 ) ;
#4730 = LINE ( 'NONE', #14103, #3220 ) ;
#4731 = SHAPE_REPRESENTATION ( '1602p_c_03', ( #12739 ), #22192 ) ;
#4732 = CARTESIAN_POINT ( 'NONE',  ( 0.000000000000000000, 2.500000000000000000, -5.000000000000000000 ) ) ;
#4733 = VERTEX_POINT ( 'NONE', #1193 ) ;
#4734 = CALENDAR_DATE ( 2026, 31, 10 ) ;
#4735 = EDGE_CURVE ( 'NONE', #2908, #1005, #1990, .T. ) ;
#4736 = EDGE_LOOP ( 'NONE', ( #13626, #20753, #18295, #4669, #13833 ) ) ;
#4737 = CARTESIAN_POINT ( 'NONE',  ( -4.514225866272930432, 4.676725866273559795, 2.500000000000000000 ) ) ;
#4738 = DIRECTION ( 'NONE',  ( 2.982858504489129897E-17, -2.441916418604790135E-15, -1.000000000000000000 ) ) ;
#4739 = ORIENTED_EDGE ( 'NONE', *, *, #17674, .F. ) ;
#4740 = CC_DESIGN_PERSON_AND_ORGANIZATION_ASSIGNMENT ( #20668, #4404, ( #7661 ) ) ;
#4741 = CARTESIAN_POINT ( 'NONE',  ( -32.64682763696299617, 7.329162855357650663, -5.000000000000000000 ) ) ;
#4742 = APPROVAL ( #7495, 'UNSPECIFIED' ) ;
#4743 = CARTESIAN_POINT ( 'NONE',  ( -32.65701080836369385, 9.273987487686079945, -5.000000000000000000 ) ) ;
#4744 = DIRECTION ( 'NONE',  ( -2.269747459788994803E-13, -2.220446049250320181E-15, -1.000000000000000000 ) ) ;
#4745 = VERTEX_POINT ( 'NONE', #1316 ) ;
#4746 = ORIENTED_EDGE ( 'NONE', *, *, #19575, .T. ) ;
#4747 = DIRECTION ( 'NONE',  ( 1.000000000000000000, -1.138590270679730064E-14, 4.484155085839414876E-45 ) ) ;
#4748 = VERTEX_POINT ( 'NONE', #23044 ) ;
#4749 = EDGE_CURVE ( 'NONE', #22247, #16889, #15268, .T. ) ;
#4750 = EDGE_CURVE ( 'NONE', #20922, #544, #5035, .T. ) ;
#4751 = DATE_AND_TIME ( #21023, #20143 ) ;
#4752 = ORIENTED_EDGE ( 'NONE', *, *, #2536, .T. ) ;
#4753 = AXIS2_PLACEMENT_3D ( 'NONE', #18878, #17076, #7946 ) ;
#4754 = EDGE_LOOP ( 'NONE', ( #13863, #18869, #4617, #2449 ) ) ;
#4755 = DIRECTION ( 'NONE',  ( -0.1997366180463770735, -0.8426774492125654881, -0.4999999999999997780 ) ) ;
#4756 = APPLICATION_PROTOCOL_DEFINITION ( 'international standard', 'config_control_design', 1994, #22004 ) ;
#4757 = DIRECTION ( 'NONE',  ( 0.9730401042858024541, -0.2306359803922080898, -5.959266323858942451E-17 ) ) ;
#4758 = APPLICATION_CONTEXT ( 'configuration controlled 3d designs of mechanical parts and assemblies' ) ;
#4759 = CYLINDRICAL_SURFACE ( 'NONE', #20988, 2.066999999999999726 ) ;
#4760 = CARTESIAN_POINT ( 'NONE',  ( -28.95596696049959817, -6.651703575491109355, 4.767474059747909720 ) ) ;
#4761 = DATE_AND_TIME ( #17359, #8362 ) ;
#4762 = EDGE_CURVE ( 'NONE', #10345, #21559, #2030, .T. ) ;
#4763 = CIRCLE ( 'NONE', #10860, 0.0009999999996440807337 ) ;
#4764 = VERTEX_POINT ( 'NONE', #1545 ) ;
#4765 = CARTESIAN_POINT ( 'NONE',  ( 58.49563186522070168, 17.70675969991889787, 13.00000000000000000 ) ) ;
#4766 = CARTESIAN_POINT ( 'NONE',  ( 55.46237324781409939, -8.294657213477510282, -13.00000000000000000 ) ) ;
#4767 = ORIENTED_EDGE ( 'NONE', *, *, #1509, .T. ) ;
#4768 = AXIS2_PLACEMENT_3D ( 'NONE', #320, #20180, #3772 ) ;
#4769 = EDGE_CURVE ( 'NONE', #5040, #21066, #12885, .T. ) ;
#4770 = CARTESIAN_POINT ( 'NONE',  ( -20.00000000397270128, 22.95208919257349933, 8.000000000004460432 ) ) ;
#4771 = LINE ( 'NONE', #16801, #18748 ) ;
#4772 = ORIENTED_EDGE ( 'NONE', *, *, #16483, .F. ) ;
#4773 = DIRECTION ( 'NONE',  ( 0.000000000000000000, -2.710505431696529444E-14, -1.000000000000000000 ) ) ;
#4774 = EDGE_CURVE ( 'NONE', #418, #560, #11070, .T. ) ;
#4775 = DATE_TIME_ROLE ( 'creation_date' ) ;
#4777 = EDGE_CURVE ( 'NONE', #12098, #11662, #7152, .T. ) ;
#4776 = ORIENTED_EDGE ( 'NONE', *, *, #801, .T. ) ;
#4778 = ORIENTED_EDGE ( 'NONE', *, *, #1483, .F. ) ;
#4779 = DIRECTION ( 'NONE',  ( 2.269747459788990007E-13, 2.220446049250330436E-15, 1.000000000000000000 ) ) ;
#4780 = CARTESIAN_POINT ( 'NONE',  ( 35.59419854219520118, 9.774809681453518806, 19.78350000000000009 ) ) ;
#4781 = SPHERICAL_SURFACE ( 'NONE', #19037, 15.25000000000000000 ) ;
#4782 = COORDINATED_UNIVERSAL_TIME_OFFSET ( 0, 0, .AHEAD. ) ;
#4783 = DIRECTION ( 'NONE',  ( 0.2306359803922080620, 0.9730401042858023430, 2.088419338574010618E-14 ) ) ;
#4784 = DIRECTION ( 'NONE',  ( -0.9730401042858022320, 0.2306359803922080343, -2.823631968772345358E-31 ) ) ;
#4785 = APPROVAL_ROLE ( '' ) ;
#4786 = FACE_OUTER_BOUND ( 'NONE', #11202, .T. ) ;
#4787 = VECTOR ( 'NONE', #3209, 1000.000000000000000 ) ;
#4788 =( NAMED_UNIT ( * ) SI_UNIT ( $, .STERADIAN. ) SOLID_ANGLE_UNIT ( ) );
#4789 = DIRECTION ( 'NONE',  ( -0.2306359803922031770, -0.9730401042858034533, 0.000000000000000000 ) ) ;
#4790 = APPROVAL_STATUS ( 'not_yet_approved' ) ;
#4791 = DIRECTION ( 'NONE',  ( 2.979206038694609145E-09, -0.4472135954999635343, -0.8944271909999130798 ) ) ;
#4792 = CARTESIAN_POINT ( 'NONE',  ( 51.98156320189720958, 17.12649442102254937, 13.00000000000000000 ) ) ;
#4793 = APPROVAL ( #19365, 'UNSPECIFIED' ) ;
#4794 = DIRECTION ( 'NONE',  ( -0.9730401042858022320, 0.2306359803922080343, 5.959266323858941219E-17 ) ) ;
#4795 = AXIS2_PLACEMENT_3D ( 'NONE', #11034, #1859, #5791 ) ;
#4796 = CARTESIAN_POINT ( 'NONE',  ( 6.500000000000000000, -1.630990338096509915E-14, 2.500000000000000000 ) ) ;
#4797 = AXIS2_PLACEMENT_3D ( 'NONE', #2953, #16635, #6285 ) ;
#4798 = CARTESIAN_POINT ( 'NONE',  ( -4.514225866272930432, 4.676725866273559795, 2.500000000000000000 ) ) ;
#4799 = EDGE_LOOP ( 'NONE', ( #3723, #5665 ) ) ;
#4800 = CARTESIAN_POINT ( 'NONE',  ( 31.49315201223960159, -2.613324229818040134, 11.84529946162094838 ) ) ;
#4801 = VERTEX_POINT ( 'NONE', #14378 ) ;
#4802 = VERTEX_POINT ( 'NONE', #114 ) ;
#4803 = FACE_OUTER_BOUND ( 'NONE', #16877, .T. ) ;
#4804 = LINE ( 'NONE', #12074, #8319 ) ;
#4805 = VERTEX_POINT ( 'NONE', #21845 ) ;
#4806 = FACE_OUTER_BOUND ( 'NONE', #7628, .T. ) ;
#4807 = VERTEX_POINT ( 'NONE', #12728 ) ;
#4808 = DIRECTION ( 'NONE',  ( -3.210834492181045054E-17, 2.441916418604790135E-15, 1.000000000000000000 ) ) ;
#4809 = APPROVAL_DATE_TIME ( #20841, #651 ) ;
#4810 = CARTESIAN_POINT ( 'NONE',  ( 96.33985310849000427, -20.10796027570521716, -13.00000000000000000 ) ) ;
#4811 = EDGE_CURVE ( 'NONE', #22224, #1981, #14781, .T. ) ;
#4812 = AXIS2_PLACEMENT_3D ( 'NONE', #4594, #2819, #7810 ) ;
#4813 = DATE_AND_TIME ( #6725, #10709 ) ;
#4814 = CIRCLE ( 'NONE', #8996, 3.500000000000001332 ) ;
#4815 = VECTOR ( 'NONE', #603, 1000.000000000000114 ) ;
#4816 =( NAMED_UNIT ( * ) PLANE_ANGLE_UNIT ( ) SI_UNIT ( $, .RADIAN. ) );
#4817 = DIRECTION ( 'NONE',  ( -3.210834492181040124E-17, 2.441916418604790135E-15, 1.000000000000000000 ) ) ;
#4818 = DIRECTION ( 'NONE',  ( -0.9730401042858022320, 0.2306359803922080343, 5.959266323858941219E-17 ) ) ;
#4819 = FACE_OUTER_BOUND ( 'NONE', #15318, .T. ) ;
#4820 = EDGE_LOOP ( 'NONE', ( #18920, #9762 ) ) ;
#4821 = DIRECTION ( 'NONE',  ( 1.000000000000000000, -1.053113628799951803E-24, -1.138589415207818163E-14 ) ) ;
#4822 = ADVANCED_BREP_SHAPE_REPRESENTATION ( '', ( #1233, #12739 ), #3270 ) ;
#4823 = CARTESIAN_POINT ( 'NONE',  ( 34.27523609350100031, 22.85428078671360197, 15.00000000000000000 ) ) ;
#4824 = VERTEX_POINT ( 'NONE', #7386 ) ;
#4825 = CIRCLE ( 'NONE', #18106, 4.349999999999976552 ) ;
#4826 = LINE ( 'NONE', #6492, #11673 ) ;
#4827 = CARTESIAN_POINT ( 'NONE',  ( -25.49858938551139786, -0.2322002804899460093, -3.750000000000000000 ) ) ;
#4828 = AXIS2_PLACEMENT_3D ( 'NONE', #12661, #6969, #23079 ) ;
#4829 = DATE_AND_TIME ( #17668, #17490 ) ;
#4830 = DIRECTION ( 'NONE',  ( -0.9730401042858024541, 0.2306359803922080898, 5.959266323858222616E-17 ) ) ;
#4831 = CIRCLE ( 'NONE', #14690, 5.000000000000000888 ) ;
#4832 = VERTEX_POINT ( 'NONE', #7041 ) ;
#4833 = VERTEX_POINT ( 'NONE', #21392 ) ;
#4834 = COORDINATED_UNIVERSAL_TIME_OFFSET ( 0, 0, .AHEAD. ) ;
#4835 = CARTESIAN_POINT ( 'NONE',  ( -20.00000000000000000, -20.00000000000000000, -2.500000000000000000 ) ) ;
#4836 = VERTEX_POINT ( 'NONE', #14260 ) ;
#4837 = DIRECTION ( 'NONE',  ( 0.000000000000000000, -1.000000000000000000, 2.081668171172169697E-15 ) ) ;
#4838 = CIRCLE ( 'NONE', #15440, 9.000000000000005329 ) ;
#4839 = COORDINATED_UNIVERSAL_TIME_OFFSET ( 0, 0, .AHEAD. ) ;
#4840 = EDGE_CURVE ( 'NONE', #4733, #12382, #2651, .T. ) ;
#4841 = PERSON_AND_ORGANIZATION_ROLE ( 'classification_officer' ) ;
#4842 = CIRCLE ( 'NONE', #2572, 2.500000000000000000 ) ;
#4843 = DIRECTION ( 'NONE',  ( 2.269747459788990007E-13, 2.220446049250330436E-15, 1.000000000000000000 ) ) ;
#4844 = CIRCLE ( 'NONE', #4083, 2.066999999999999726 ) ;
#4845 = AXIS2_PLACEMENT_3D ( 'NONE', #12090, #6731, #13852 ) ;
#4846 = DIRECTION ( 'NONE',  ( -4.028143194477080210E-16, -2.054129435991050111E-15, -1.000000000000000000 ) ) ;
#4847 = ORIENTED_EDGE ( 'NONE', *, *, #5199, .T. ) ;
#4848 = EDGE_CURVE ( 'NONE', #10218, #23033, #21498, .T. ) ;
#4849 = EDGE_CURVE ( 'NONE', #17240, #11373, #20850, .T. ) ;
#4850 = VERTEX_POINT ( 'NONE', #3790 ) ;
#4851 = VECTOR ( 'NONE', #10327, 1000.000000000000227 ) ;
#4852 = DIRECTION ( 'NONE',  ( 0.9730401042858035643, -0.2306359803922028717, -5.432877459303547053E-17 ) ) ;
#4853 = LINE ( 'NONE', #23117, #12788 ) ;
#4854 = ORIENTED_EDGE ( 'NONE', *, *, #6545, .F. ) ;
#4855 = LINE ( 'NONE', #6402, #17384 ) ;
#4856 = DIRECTION ( 'NONE',  ( 6.123230159571619958E-17, 0.000000000000000000, 1.000000000000000000 ) ) ;
#4857 = EDGE_CURVE ( 'NONE', #19671, #3674, #9868, .T. ) ;
#4858 = CARTESIAN_POINT ( 'NONE',  ( -59.87132660632070014, -21.81388311970430038, 5.000000000000000000 ) ) ;
#4859 = AXIS2_PLACEMENT_3D ( 'NONE', #13036, #17046, #11509 ) ;
#4860 = ORIENTED_EDGE ( 'NONE', *, *, #3941, .T. ) ;
#4861 = ORIENTED_EDGE ( 'NONE', *, *, #9372, .T. ) ;
#4862 = CARTESIAN_POINT ( 'NONE',  ( -20.00000000000130029, -20.00000000000000000, -5.499999999995469402 ) ) ;
#4863 = ORIENTED_EDGE ( 'NONE', *, *, #12261, .F. ) ;
#4864 = CALENDAR_DATE ( 2026, 31, 10 ) ;
#4865 = ORIENTED_EDGE ( 'NONE', *, *, #13206, .T. ) ;
#4866 = ORIENTED_EDGE ( 'NONE', *, *, #1482, .T. ) ;
#4867 = DIRECTION ( 'NONE',  ( -0.9080662505692100872, 0.4188265566761218417, -1.040834085574018826E-15 ) ) ;
#4868 = VECTOR ( 'NONE', #3701, 1000.000000000000000 ) ;
#4869 = APPROVAL_STATUS ( 'not_yet_approved' ) ;
#4870 = EDGE_CURVE ( 'NONE', #22602, #23272, #9634, .T. ) ;
#4871 = DIRECTION ( 'NONE',  ( -0.9730401042858022320, 0.2306359803922080343, 5.959266323858941219E-17 ) ) ;
#4872 =( BOUNDED_CURVE ( )  B_SPLINE_CURVE ( 2, ( #9178, #1569, #137 ),
 .UNSPECIFIED., .F., .F. ) 
 B_SPLINE_CURVE_WITH_KNOTS ( ( 3, 3 ),
 ( 0.000000000000000000, 0.2336872276155859962 ),
 .UNSPECIFIED. ) 
 CURVE ( )  GEOMETRIC_REPRESENTATION_ITEM ( )  RATIONAL_B_SPLINE_CURVE ( ( 1.000000000000000000, 1.154700538379259900, 1.000000000000000000 ) ) 
 REPRESENTATION_ITEM ( '' )  );
#4873 = CC_DESIGN_DATE_AND_TIME_ASSIGNMENT ( #13491, #22031, ( #9078 ) ) ;
#4874 = EDGE_CURVE ( 'NONE', #1296, #12606, #12167, .T. ) ;
#4875 = CC_DESIGN_PERSON_AND_ORGANIZATION_ASSIGNMENT ( #19209, #22990, ( #7215 ) ) ;
#4876 =( NAMED_UNIT ( * ) SI_UNIT ( $, .STERADIAN. ) SOLID_ANGLE_UNIT ( ) );
#4877 = FACE_BOUND ( 'NONE', #12406, .T. ) ;
#4878 = ADVANCED_FACE ( 'NONE', ( #19726 ), #10726, .F. ) ;
#4879 = EDGE_CURVE ( 'NONE', #12948, #11681, #18597, .T. ) ;
#4880 = CARTESIAN_POINT ( 'NONE',  ( 34.88044566782584610, 28.44271146055880095, -18.00000000000029843 ) ) ;
#4881 = PERSON_AND_ORGANIZATION ( #11966, #8758 ) ;
#4882 = PRODUCT_DEFINITION ( 'UNKNOWN', '', #3780, #15632 ) ;
#4883 = VECTOR ( 'NONE', #5904, 1000.000000000000114 ) ;
#4884 = ORIENTED_EDGE ( 'NONE', *, *, #8732, .F. ) ;
#4885 = LINE ( 'NONE', #20909, #1150 ) ;
#4886 = CARTESIAN_POINT ( 'NONE',  ( 5.000000000000000000, -27.34999999999999787, 6.250000000000000000 ) ) ;
#4887 = ORIENTED_EDGE ( 'NONE', *, *, #19403, .T. ) ;
#4888 = DIRECTION ( 'NONE',  ( -0.9999862922474493931, -0.005235963827116132258, -3.478334803857182996E-33 ) ) ;
#4889 = DIRECTION ( 'NONE',  ( -2.979184025347991663E-09, 0.4472135954999659213, 0.8944271909999118586 ) ) ;
#4890 = DIRECTION ( 'NONE',  ( 0.2306359803922094498, 0.9730401042858018990, 0.000000000000000000 ) ) ;
#4891 = ORIENTED_EDGE ( 'NONE', *, *, #20493, .F. ) ;
#4892 = CARTESIAN_POINT ( 'NONE',  ( 33.27705887009690144, -3.036156860537079893, 13.00000000000019895 ) ) ;
#4893 = COORDINATED_UNIVERSAL_TIME_OFFSET ( 0, 0, .AHEAD. ) ;
#4894 = VERTEX_POINT ( 'NONE', #21737 ) ;
#4895 = ORIENTED_EDGE ( 'NONE', *, *, #14177, .T. ) ;
#4896 = CARTESIAN_POINT ( 'NONE',  ( -27.00000000000000000, -28.60000000000000142, 6.250000000000000000 ) ) ;
#4897 = CARTESIAN_POINT ( 'NONE',  ( -65.82123935389580538, 11.86253283145240012, 5.000000000000000000 ) ) ;
#4898 = DIRECTION ( 'NONE',  ( 0.000000000000000000, 1.000000000000000000, 0.000000000000000000 ) ) ;
#4899 = SHAPE_DEFINITION_REPRESENTATION ( #5301, #12037 ) ;
#4900 = CARTESIAN_POINT ( 'NONE',  ( 36.76922337734895052, -6.947011889080550340, -20.00000000000000000 ) ) ;
#4901 = EDGE_CURVE ( 'NONE', #2029, #12414, #10959, .T. ) ;
#4902 = DIRECTION ( 'NONE',  ( 0.9286452767786566032, 1.871119812896368998E-17, -0.3709689338970208472 ) ) ;
#4903 = DIRECTION ( 'NONE',  ( -3.469446951953605354E-14, -1.084202172485501657E-13, 1.000000000000000000 ) ) ;
#4904 = SHAPE_REPRESENTATION_RELATIONSHIP ( 'NONE' , 'NONE' ,  #1388, #10524 ) ;
#4905 = AXIS2_PLACEMENT_3D ( 'NONE', #6717, #13948, #21184 ) ;
#4906 = EDGE_CURVE ( 'NONE', #20851, #10381, #16390, .T. ) ;
#4907 = DIRECTION ( 'NONE',  ( -1.000000000000000000, 2.270069654138870255E-15, 0.000000000000000000 ) ) ;
#4908 = APPLICATION_PROTOCOL_DEFINITION ( 'international standard', 'config_control_design', 1994, #3050 ) ;
#4909 = EDGE_CURVE ( 'NONE', #5883, #15816, #5673, .T. ) ;
#4910 = DIRECTION ( 'NONE',  ( 0.2306359803922085339, 0.9730401042858022320, 0.000000000000000000 ) ) ;
#4911 = CARTESIAN_POINT ( 'NONE',  ( -14.00000000000180123, -19.99999999944489915, -7.999999999996829203 ) ) ;
#4912 = DIRECTION ( 'NONE',  ( 0.2306359803922085339, 0.9730401042858022320, 0.000000000000000000 ) ) ;
#4913 = CARTESIAN_POINT ( 'NONE',  ( 35.59419854219520118, 9.774809681453550780, 26.88000000000000256 ) ) ;
#4914 = DIRECTION ( 'NONE',  ( 0.9730401042858035643, -0.2306359803922028717, -5.959266323858677443E-17 ) ) ;
#4915 = ORIENTED_EDGE ( 'NONE', *, *, #11446, .F. ) ;
#4916 = DIRECTION ( 'NONE',  ( -3.099353312215989243E-62, 0.000000000000000000, 1.000000000000000000 ) ) ;
#4917 = UNCERTAINTY_MEASURE_WITH_UNIT (LENGTH_MEASURE( 1.000000000000000082E-05 ), #35, 'distance_accuracy_value', 'NONE');
#4918 = VERTEX_POINT ( 'NONE', #7965 ) ;
#4919 = PRODUCT ( '1602p_c_08', '1602p_c_08', '', ( #15428 ) ) ;
#4920 = ORIENTED_EDGE ( 'NONE', *, *, #13173, .T. ) ;
#4921 = DIRECTION ( 'NONE',  ( -3.099353312215988811E-62, 0.000000000000000000, 1.000000000000000000 ) ) ;
#4922 = CARTESIAN_POINT ( 'NONE',  ( 43.84419854219520829, -33.09999999999998721, -25.00000000000000000 ) ) ;
#4923 = ORIENTED_EDGE ( 'NONE', *, *, #18232, .F. ) ;
#4924 = ORIENTED_EDGE ( 'NONE', *, *, #2972, .T. ) ;
#4925 = VECTOR ( 'NONE', #18180, 1000.000000000000227 ) ;
#4926 = DIRECTION ( 'NONE',  ( -0.9730401042858024541, 0.2306359803922080898, 5.959266323858711956E-17 ) ) ;
#4927 = ORIENTED_EDGE ( 'NONE', *, *, #9729, .T. ) ;
#4928 = DIRECTION ( 'NONE',  ( -0.9730401042858036753, 0.2306359803922031493, 5.432877459303543355E-17 ) ) ;
#4929 = AXIS2_PLACEMENT_3D ( 'NONE', #23216, #4943, #17883 ) ;
#4930 = CALENDAR_DATE ( 2026, 31, 10 ) ;
#4931 = CONTEXT_DEPENDENT_SHAPE_REPRESENTATION ( #3552, #9303 ) ;
#4932 = ADVANCED_FACE ( 'NONE', ( #22079 ), #2616, .F. ) ;
#4933 = DIRECTION ( 'NONE',  ( -6.662112528310618598E-09, 1.000000000000000000, -2.081668171172169697E-15 ) ) ;
#4934 = EDGE_CURVE ( 'NONE', #17992, #341, #22739, .T. ) ;
#4935 = DIRECTION ( 'NONE',  ( -6.662112528310618598E-09, 1.000000000000000000, -2.081668171172169697E-15 ) ) ;
#4936 = LOCAL_TIME ( 14, 11, 27.00000000000000000, #19837 ) ;
#4937 = AXIS2_PLACEMENT_3D ( 'NONE', #16307, #8967, #7301 ) ;
#4938 = DIRECTION ( 'NONE',  ( -0.9997648975362233292, -0.02168293463498010415, 0.000000000000000000 ) ) ;
#4939 = AXIS2_PLACEMENT_3D ( 'NONE', #19474, #6528, #19349 ) ;
#4940 = ORIENTED_EDGE ( 'NONE', *, *, #13911, .F. ) ;
#4941 = DIRECTION ( 'NONE',  ( 0.000000000000000000, -1.000000000000000000, 2.081668171172168119E-15 ) ) ;
#4942 = DESIGN_CONTEXT ( 'detailed design', #19912, 'design' ) ;
#4943 = DIRECTION ( 'NONE',  ( -0.9730401042858024541, 0.2306359803922080898, 5.959266323858952312E-17 ) ) ;
#4944 = ORIENTED_EDGE ( 'NONE', *, *, #5037, .F. ) ;
#4945 = CARTESIAN_POINT ( 'NONE',  ( 33.61438040303559660, 10.38400890524524023, -8.999987531128509133 ) ) ;
#4946 = CARTESIAN_POINT ( 'NONE',  ( 52.26033179423370001, -7.535689554643980159, -13.00000000000039968 ) ) ;
#4947 = VECTOR ( 'NONE', #9415, 1000.000000000000114 ) ;
#4948 = ORIENTED_EDGE ( 'NONE', *, *, #5679, .T. ) ;
#4949 = APPROVAL_STATUS ( 'not_yet_approved' ) ;
#4950 = DIRECTION ( 'NONE',  ( 0.9286452767786566032, 1.871119812896368998E-17, -0.3709689338970208472 ) ) ;
#4951 = VECTOR ( 'NONE', #21621, 999.9999999999998863 ) ;
#4952 = ORIENTED_EDGE ( 'NONE', *, *, #8689, .T. ) ;
#4953 = ORIENTED_EDGE ( 'NONE', *, *, #17226, .F. ) ;
#4954 = APPROVAL_STATUS ( 'not_yet_approved' ) ;
#4955 = DIRECTION ( 'NONE',  ( -0.2306359803922030105, -0.9730401042858034533, 0.000000000000000000 ) ) ;
#4956 = VERTEX_POINT ( 'NONE', #15080 ) ;
#4957 = LOCAL_TIME ( 14, 11, 27.00000000000000000, #9870 ) ;
#4958 = DIRECTION ( 'NONE',  ( 0.000000000000000000, 0.000000000000000000, -1.000000000000000000 ) ) ;
#4959 = AXIS2_PLACEMENT_3D ( 'NONE', #8389, #10190, #6842 ) ;
#4960 = APPROVAL_ROLE ( '' ) ;
#4961 = PERSON_AND_ORGANIZATION ( #8783, #10328 ) ;
#4962 = CARTESIAN_POINT ( 'NONE',  ( 36.17078849317570644, 12.20740994216783726, -17.70000000000051088 ) ) ;
#4963 = CARTESIAN_POINT ( 'NONE',  ( -20.00000000000130029, -20.00000000000000000, -5.499999999995469402 ) ) ;
#4964 = ORIENTED_EDGE ( 'NONE', *, *, #11294, .T. ) ;
#4965 = CC_DESIGN_SECURITY_CLASSIFICATION ( #6120, ( #7624 ) ) ;
#4966 = ORIENTED_EDGE ( 'NONE', *, *, #13009, .T. ) ;
#4967 = APPROVAL_PERSON_ORGANIZATION ( #11302, #17515, #7482 ) ;
#4968 = DIRECTION ( 'NONE',  ( 0.000000000000000000, 1.000000000000000000, -9.248937406224699144E-11 ) ) ;
#4969 = PLANE ( 'NONE',  #3668 ) ;
#4971 = EDGE_LOOP ( 'NONE', ( #20897, #10976 ) ) ;
#4970 = EDGE_CURVE ( 'NONE', #11110, #19959, #1875, .T. ) ;
#4972 = AXIS2_PLACEMENT_3D ( 'NONE', #9727, #8284, #6021 ) ;
#4973 = ADVANCED_FACE ( 'NONE', ( #14965 ), #22437, .F. ) ;
#4974 = SECURITY_CLASSIFICATION ( '', '', #21095 ) ;
#4975 = CARTESIAN_POINT ( 'NONE',  ( 45.07211867146960316, 28.08243186520980217, -10.02499999999999858 ) ) ;
#4976 = LINE ( 'NONE', #18890, #11134 ) ;
#4977 = ORIENTED_EDGE ( 'NONE', *, *, #3854, .F. ) ;
#4978 = APPROVAL_PERSON_ORGANIZATION ( #3060, #14439, #5091 ) ;
#4979 = ORIENTED_EDGE ( 'NONE', *, *, #7066, .T. ) ;
#4980 = CARTESIAN_POINT ( 'NONE',  ( 39.83668191656649782, 5.994421497922090225, -18.89999999999999858 ) ) ;
#4981 = EDGE_LOOP ( 'NONE', ( #12812, #13566, #4487, #11197 ) ) ;
#4982 = AXIS2_PLACEMENT_3D ( 'NONE', #3852, #7319, #14559 ) ;
#4983 = COORDINATED_UNIVERSAL_TIME_OFFSET ( 0, 0, .AHEAD. ) ;
#4984 = ORIENTED_EDGE ( 'NONE', *, *, #20099, .F. ) ;
#4985 = ORIENTED_EDGE ( 'NONE', *, *, #23434, .T. ) ;
#4986 = CARTESIAN_POINT ( 'NONE',  ( 35.34171762861019772, 30.38879166913045182, -16.00000000000029843 ) ) ;
#4987 = COORDINATED_UNIVERSAL_TIME_OFFSET ( 0, 0, .AHEAD. ) ;
#4988 = EDGE_CURVE ( 'NONE', #2417, #20341, #11203, .T. ) ;
#4989 = LOCAL_TIME ( 14, 11, 27.00000000000000000, #2772 ) ;
#4990 = CARTESIAN_POINT ( 'NONE',  ( -55.83667484026289429, -6.792351917569590114, -7.200000000000000178 ) ) ;
#4991 = LOCAL_TIME ( 14, 11, 27.00000000000000000, #11573 ) ;
#4992 = CIRCLE ( 'NONE', #20917, 2.066999999999999726 ) ;
#4993 = ORGANIZATION ( 'NAUO-ORG22', 'UNSPECIFIED', 'UNSPECIFIED' ) ;
#4994 = FACE_OUTER_BOUND ( 'NONE', #12590, .T. ) ;
#4995 = PERSON_AND_ORGANIZATION_ROLE ( 'design_supplier' ) ;
#4996 = ORIENTED_EDGE ( 'NONE', *, *, #21881, .T. ) ;
#4997 = CARTESIAN_POINT ( 'NONE',  ( 103.2898377416287303, 9.213630226843287474, -13.00000000000000000 ) ) ;
#4998 = CARTESIAN_POINT ( 'NONE',  ( 28.41185834866789861, -1.882976958576189963, -13.00000000000039968 ) ) ;
#4999 = VERTEX_POINT ( 'NONE', #22198 ) ;
#5000 = EDGE_CURVE ( 'NONE', #18569, #8287, #4397, .T. ) ;
#5001 = SECURITY_CLASSIFICATION ( '', '', #11671 ) ;
#5002 = CARTESIAN_POINT ( 'NONE',  ( -29.94163891957289891, 6.343422587376370103, 3.750000000000000000 ) ) ;
#5003 = DIRECTION ( 'NONE',  ( 0.2306359803922080898, 0.9730401042858024541, -2.572202231434325988E-16 ) ) ;
#5004 = CARTESIAN_POINT ( 'NONE',  ( 37.01481097301077483, 22.79827665208033238, 15.00000000000000355 ) ) ;
#5005 = ORIENTED_EDGE ( 'NONE', *, *, #9084, .T. ) ;
#5006 = CARTESIAN_POINT ( 'NONE',  ( 39.27359436029429673, 22.26288585089420025, -16.37500000000050093 ) ) ;
#5007 = CIRCLE ( 'NONE', #22061, 2.009239999999998805 ) ;
#5008 = CC_DESIGN_DATE_AND_TIME_ASSIGNMENT ( #18410, #1649, ( #18177 ) ) ;
#5009 = PERSON_AND_ORGANIZATION_ROLE ( 'creator' ) ;
#5010 = EDGE_LOOP ( 'NONE', ( #4008, #15017 ) ) ;
#5011 = PRODUCT_RELATED_PRODUCT_CATEGORY ( 'detail', '', ( #4728 ) ) ;
#5012 = ORIENTED_EDGE ( 'NONE', *, *, #18439, .F. ) ;
#5013 = DIRECTION ( 'NONE',  ( 1.224646799147353207E-16, 1.000000000000000000, -0.000000000000000000 ) ) ;
#5014 = DIRECTION ( 'NONE',  ( 1.000000000000000000, 0.000000000000000000, 1.480297366166879989E-16 ) ) ;
#5015 = CC_DESIGN_APPROVAL ( #15302, ( #18637 ) ) ;
#5016 = LINE ( 'NONE', #19273, #14852 ) ;
#5017 = PERSON_AND_ORGANIZATION ( #11966, #8758 ) ;
#5018 = EDGE_CURVE ( 'NONE', #7920, #5108, #14725, .T. ) ;
#5019 = CARTESIAN_POINT ( 'NONE',  ( -19.99975861755289941, 22.95209442650110176, 5.000000000000000000 ) ) ;
#5020 = EDGE_CURVE ( 'NONE', #23452, #16466, #7964, .T. ) ;
#5021 = CARTESIAN_POINT ( 'NONE',  ( -20.00000000000000000, -20.00000000000000000, 5.500000000004559020 ) ) ;
#5022 = AXIS2_PLACEMENT_3D ( 'NONE', #1784, #14385, #21615 ) ;
#5023 = CARTESIAN_POINT ( 'NONE',  ( 117.1241794131700118, -12.63305097454430026, 15.90000000000000036 ) ) ;
#5024 = APPROVAL_PERSON_ORGANIZATION ( #6275, #10427, #7705 ) ;
#5025 = CARTESIAN_POINT ( 'NONE',  ( 0.000000000000000000, 0.000000000000000000, 0.000000000000000000 ) ) ;
#5026 = CIRCLE ( 'NONE', #9598, 2.500000000000001776 ) ;
#5027 = AXIS2_PLACEMENT_3D ( 'NONE', #11962, #15957, #17752 ) ;
#5028 = ORIENTED_EDGE ( 'NONE', *, *, #14601, .F. ) ;
#5029 = CARTESIAN_POINT ( 'NONE',  ( -20.00000000000000000, -15.00000000000000000, -4.999999999995480060 ) ) ;
#5030 = PERSON_AND_ORGANIZATION_ROLE ( 'design_owner' ) ;
#5031 = CIRCLE ( 'NONE', #74, 8.000000000000000000 ) ;
#5032 = CARTESIAN_POINT ( 'NONE',  ( 37.65606570105540385, 9.973062512861897488, 8.976009386856667049 ) ) ;
#5033 = CYLINDRICAL_SURFACE ( 'NONE', #22240, 2.750000000000000888 ) ;
#5034 = APPLICATION_CONTEXT ( 'configuration controlled 3d designs of mechanical parts and assemblies' ) ;
#5035 = CIRCLE ( 'NONE', #23207, 7.000000000000004441 ) ;
#5036 = FACE_OUTER_BOUND ( 'NONE', #10525, .T. ) ;
#5037 = EDGE_CURVE ( 'NONE', #3254, #9785, #11007, .T. ) ;
#5038 = CARTESIAN_POINT ( 'NONE',  ( -62.82872441665799101, -8.329083101359751495, -5.528360538656857483E-15 ) ) ;
#5039 = CARTESIAN_POINT ( 'NONE',  ( -20.00000000000000000, -20.00000000000000000, 0.000000000000000000 ) ) ;
#5040 = VERTEX_POINT ( 'NONE', #5937 ) ;
#5041 = DIRECTION ( 'NONE',  ( 0.000000000000000000, 0.000000000000000000, -1.000000000000000000 ) ) ;
#5042 = PRODUCT_DEFINITION ( 'UNKNOWN', '', #6911, #1363 ) ;
#5043 = LOCAL_TIME ( 14, 11, 27.00000000000000000, #11843 ) ;
#5044 = CC_DESIGN_PERSON_AND_ORGANIZATION_ASSIGNMENT ( #10112, #15680, ( #13884 ) ) ;
#5045 = ORIENTED_EDGE ( 'NONE', *, *, #22019, .T. ) ;
#5046 = CARTESIAN_POINT ( 'NONE',  ( -26.68810977484059777, -6.639828994528159889, -2.500000000000090150 ) ) ;
#5047 = DIRECTION ( 'NONE',  ( -2.269700743865584947E-13, -2.220446049247695246E-15, -1.000000000000000000 ) ) ;
#5048 = ORIENTED_EDGE ( 'NONE', *, *, #3849, .T. ) ;
#5049 = AXIS2_PLACEMENT_3D ( 'NONE', #458, #11200, #7840 ) ;
#5050 = EDGE_CURVE ( 'NONE', #20682, #16704, #731, .T. ) ;
#5051 = VECTOR ( 'NONE', #4190, 999.9999999999998863 ) ;
#5052 = LINE ( 'NONE', #22964, #3151 ) ;
#5053 = EDGE_CURVE ( 'NONE', #19134, #2851, #12529, .T. ) ;
#5054 = ORIENTED_EDGE ( 'NONE', *, *, #18407, .F. ) ;
#5055 = VECTOR ( 'NONE', #2559, 1000.000000000000000 ) ;
#5056 = LINE ( 'NONE', #12415, #9108 ) ;
#5057 = DIRECTION ( 'NONE',  ( -5.964507377817349415E-17, -4.861311874385510251E-15, -1.000000000000000000 ) ) ;
#5058 =( NAMED_UNIT ( * ) SI_UNIT ( $, .STERADIAN. ) SOLID_ANGLE_UNIT ( ) );
#5060 = CARTESIAN_POINT ( 'NONE',  ( 118.5079952955230027, -6.794810348829399160, 15.50000000000000000 ) ) ;
#5059 = AXIS2_PLACEMENT_3D ( 'NONE', #4963, #21007, #1625 ) ;
#5061 = CARTESIAN_POINT ( 'NONE',  ( -20.00000000000140332, -20.00000000000000000, -5.499999999995469402 ) ) ;
#5062 =( LENGTH_UNIT ( ) NAMED_UNIT ( * ) SI_UNIT ( .MILLI., .METRE. ) );
#5063 = SECURITY_CLASSIFICATION ( '', '', #10420 ) ;
#5064 = CARTESIAN_POINT ( 'NONE',  ( -20.00000000000180123, -20.00000000000000000, -7.999999999995458744 ) ) ;
#5065 = VECTOR ( 'NONE', #19782, 999.9999999999998863 ) ;
#5066 = VERTEX_POINT ( 'NONE', #11426 ) ;
#5067 = CARTESIAN_POINT ( 'NONE',  ( 36.68971944905818816, 14.39675017681111058, 26.87999999999997769 ) ) ;
#5068 = AXIS2_PLACEMENT_3D ( 'NONE', #13683, #19041, #1436 ) ;
#5069 = ADVANCED_FACE ( 'NONE', ( #2376, #5691, #12947 ), #9647, .F. ) ;
#5070 = AXIS2_PLACEMENT_3D ( 'NONE', #14163, #22821, #19168 ) ;
#5071 = CARTESIAN_POINT ( 'NONE',  ( -62.91413607658799378, 7.983193290926558383, 2.191364059223300011E-15 ) ) ;
#5072 = ORIENTED_EDGE ( 'NONE', *, *, #13795, .T. ) ;
#5073 = DIRECTION ( 'NONE',  ( -0.5000051404512463327, 0.000000000000000000, 0.8660224359231865066 ) ) ;
#5074 = CARTESIAN_POINT ( 'NONE',  ( 34.85715660638717139, 8.407947612062324438, 27.55602540378454535 ) ) ;
#5075 = ORIENTED_EDGE ( 'NONE', *, *, #12480, .F. ) ;
#5076 = EDGE_CURVE ( 'NONE', #503, #8379, #18659, .T. ) ;
#5077 = CONTEXT_DEPENDENT_SHAPE_REPRESENTATION ( #8518, #10888 ) ;
#5078 = CARTESIAN_POINT ( 'NONE',  ( 113.2956221386590130, -28.78551670568859677, -3.100000000000000089 ) ) ;
#5079 = VERTEX_POINT ( 'NONE', #18544 ) ;
#5080 = VECTOR ( 'NONE', #3091, 1000.000000000000000 ) ;
#5081 = ORIENTED_EDGE ( 'NONE', *, *, #18496, .F. ) ;
#5082 = ADVANCED_FACE ( 'NONE', ( #2249 ), #16732, .T. ) ;
#5083 = APPROVAL_STATUS ( 'not_yet_approved' ) ;
#5084 = CARTESIAN_POINT ( 'NONE',  ( -55.83667431666650316, -6.792451916198809947, 7.200000000000000178 ) ) ;
#5085 = VECTOR ( 'NONE', #12689, 999.9999999999998863 ) ;
#5086 = ORIENTED_EDGE ( 'NONE', *, *, #351, .T. ) ;
#5087 = EDGE_CURVE ( 'NONE', #7660, #3931, #8725, .T. ) ;
#5088 = DIRECTION ( 'NONE',  ( 0.000000000000000000, 3.261507856373309729E-31, 1.000000000000000000 ) ) ;
#5089 = PERSON_AND_ORGANIZATION_ROLE ( 'design_owner' ) ;
#5090 = CIRCLE ( 'NONE', #18360, 2.999999999999999556 ) ;
#5091 = APPROVAL_ROLE ( '' ) ;
#5092 = LINE ( 'NONE', #4962, #16485 ) ;
#5093 = LINE ( 'NONE', #13764, #21361 ) ;
#5094 = EDGE_LOOP ( 'NONE', ( #1668, #15648, #3689, #15305 ) ) ;
#5095 = AXIS2_PLACEMENT_3D ( 'NONE', #15121, #4442, #22593 ) ;
#5096 = ORIENTED_EDGE ( 'NONE', *, *, #20411, .F. ) ;
#5097 = AXIS2_PLACEMENT_3D ( 'NONE', #10693, #7013, #5318 ) ;
#5098 = CYLINDRICAL_SURFACE ( 'NONE', #15227, 2.500000000000000444 ) ;
#5099 = CARTESIAN_POINT ( 'NONE',  ( -22.74999999999852918, -20.00000000000000000, 8.500000000005176304 ) ) ;
#5100 = ORIENTED_EDGE ( 'NONE', *, *, #8670, .T. ) ;
#5101 = APPROVAL ( #16657, 'UNSPECIFIED' ) ;
#5102 = DIRECTION ( 'NONE',  ( -0.2306359803922101992, -0.9730401042858018990, 4.616450158279816491E-15 ) ) ;
#5103 = DIRECTION ( 'NONE',  ( 0.000000000000000000, 0.000000000000000000, 1.000000000000000000 ) ) ;
#5104 = ORIENTED_EDGE ( 'NONE', *, *, #752, .T. ) ;
#5105 = ORIENTED_EDGE ( 'NONE', *, *, #9354, .T. ) ;
#5106 = VERTEX_POINT ( 'NONE', #19004 ) ;
#5107 = PERSON_AND_ORGANIZATION ( #11966, #8758 ) ;
#5108 = VERTEX_POINT ( 'NONE', #1167 ) ;
#5109 = VERTEX_POINT ( 'NONE', #8088 ) ;
#5110 = CARTESIAN_POINT ( 'NONE',  ( -70.63306599754589854, 6.130251853413639651, 5.500000000000099476 ) ) ;
#5111 = SECURITY_CLASSIFICATION_LEVEL ( 'unclassified' ) ;
#5112 = DIRECTION ( 'NONE',  ( -6.123237831918399306E-17, 1.590047762086094914E-30, 1.000000000000000000 ) ) ;
#5113 = EDGE_CURVE ( 'NONE', #3781, #4635, #11778, .T. ) ;
#5114 =( LENGTH_UNIT ( ) NAMED_UNIT ( * ) SI_UNIT ( .MILLI., .METRE. ) );
#5115 = CARTESIAN_POINT ( 'NONE',  ( -62.99678855639989905, 23.76850991288289805, 6.352789585277969841E-15 ) ) ;
#5116 = PERSON_AND_ORGANIZATION ( #11966, #8758 ) ;
#5117 = PRODUCT ( '1602p_c_36', '1602p_c_36', '', ( #23378 ) ) ;
#5118 = EDGE_LOOP ( 'NONE', ( #13686, #437 ) ) ;
#5119 = CARTESIAN_POINT ( 'NONE',  ( 105.8171986446039909, -20.23006919877430221, 13.00000000000000000 ) ) ;
#5120 = DIRECTION ( 'NONE',  ( 8.274327508162393116E-31, 2.054129435991050111E-15, 1.000000000000000000 ) ) ;
#5121 = EDGE_LOOP ( 'NONE', ( #17058, #23390, #16381, #7156 ) ) ;
#5122 = PERSON ( 'NAUO-PER8', 'UNSPECIFIED', 'UNSPECIFIED', ('UNSPECIFIED'), ('UNSPECIFIED'), ('UNSPECIFIED') ) ;
#5123 = PLANE ( 'NONE',  #7490 ) ;
#5124 = AXIS2_PLACEMENT_3D ( 'NONE', #18642, #2356, #6278 ) ;
#5125 = CARTESIAN_POINT ( 'NONE',  ( -19.99999999999999645, -15.00000000000000000, 5.500000000004549250 ) ) ;
#5126 = CARTESIAN_POINT ( 'NONE',  ( -26.75617730459320143, 6.359992804688050505, -2.500999999999729884 ) ) ;
#5127 = ORIENTED_EDGE ( 'NONE', *, *, #8767, .T. ) ;
#5128 = EDGE_LOOP ( 'NONE', ( #18873, #5468, #7997, #11045, #9308, #2818, #22170, #22633 ) ) ;
#5129 = DIRECTION ( 'NONE',  ( -0.005235963827121952255, 0.9999862922474493931, -2.738476122049126182E-14 ) ) ;
#5130 = DATE_AND_TIME ( #21045, #22769 ) ;
#5131 = ORIENTED_EDGE ( 'NONE', *, *, #10292, .T. ) ;
#5132 = ORIENTED_EDGE ( 'NONE', *, *, #15395, .T. ) ;
#5133 = FACE_OUTER_BOUND ( 'NONE', #4565, .T. ) ;
#5134 = DIRECTION ( 'NONE',  ( -0.9730401042858036753, 0.2306359803922028995, 5.958148513035547083E-17 ) ) ;
#5135 = APPROVAL_ROLE ( '' ) ;
#5136 = FACE_OUTER_BOUND ( 'NONE', #6989, .T. ) ;
#5137 = CARTESIAN_POINT ( 'NONE',  ( -17.50034580627744063, 23.00627559326238369, 4.999999999999900524 ) ) ;
#5138 = EDGE_CURVE ( 'NONE', #418, #13752, #11777, .T. ) ;
#5139 = CARTESIAN_POINT ( 'NONE',  ( 0.000000000000000000, 0.000000000000000000, 0.000000000000000000 ) ) ;
#5140 = CC_DESIGN_PERSON_AND_ORGANIZATION_ASSIGNMENT ( #194, #11174, ( #10735 ) ) ;
#5141 = DIRECTION ( 'NONE',  ( 0.2306359803922080898, 0.9730401042858024541, -2.572202231434325988E-16 ) ) ;
#5142 = COORDINATED_UNIVERSAL_TIME_OFFSET ( 0, 0, .AHEAD. ) ;
#5143 = DIRECTION ( 'NONE',  ( -0.8823529412199648814, 0.4705882352125658197, 9.020562075079400046E-15 ) ) ;
#5144 = DIRECTION ( 'NONE',  ( -9.248890187689720549E-11, 1.000000000000000000, -2.220446048198180498E-15 ) ) ;
#5145 = EDGE_CURVE ( 'NONE', #6789, #9680, #15547, .T. ) ;
#5146 = EDGE_CURVE ( 'NONE', #18183, #22408, #19235, .T. ) ;
#5147 = CARTESIAN_POINT ( 'NONE',  ( 36.50043006307940630, 22.92019839501199741, -13.00000000000030020 ) ) ;
#5148 = VERTEX_POINT ( 'NONE', #13534 ) ;
#5149 = DIRECTION ( 'NONE',  ( 0.000000000000000000, 0.000000000000000000, 1.000000000000000000 ) ) ;
#5150 = ORIENTED_EDGE ( 'NONE', *, *, #9230, .T. ) ;
#5151 = CARTESIAN_POINT ( 'NONE',  ( 1.133770560463819718E-13, -8.411617717272179750E-16, 8.874009851233079243E-14 ) ) ;
#5152 = FACE_OUTER_BOUND ( 'NONE', #3876, .T. ) ;
#5153 = ORIENTED_EDGE ( 'NONE', *, *, #16481, .T. ) ;
#5154 = CARTESIAN_POINT ( 'NONE',  ( 117.1011158151309957, -12.73035498497280038, 20.00000000000000000 ) ) ;
#5155 = TOROIDAL_SURFACE ( 'NONE', #18443, 3.750000000000000000, 0.5000000000000000000 ) ;
#5156 = ORIENTED_EDGE ( 'NONE', *, *, #11761, .T. ) ;
#5157 = DIRECTION ( 'NONE',  ( 0.9730401042858035643, -0.2306359803922029272, 1.531342102931249911E-15 ) ) ;
#5158 = CALENDAR_DATE ( 2026, 31, 10 ) ;
#5159 = CARTESIAN_POINT ( 'NONE',  ( 39.76749112244880280, 5.702509466636288771, 15.90000000000000036 ) ) ;
#5160 = EDGE_CURVE ( 'NONE', #21777, #22844, #7220, .T. ) ;
#5161 =( NAMED_UNIT ( * ) PLANE_ANGLE_UNIT ( ) SI_UNIT ( $, .RADIAN. ) );
#5162 = CARTESIAN_POINT ( 'NONE',  ( -23.50000000000000000, -20.00000000000000000, -5.000000000000000000 ) ) ;
#5163 = APPROVAL ( #14678, 'UNSPECIFIED' ) ;
#5164 = CARTESIAN_POINT ( 'NONE',  ( 35.59419854219520118, 9.774809681453239918, -37.44562646538079775 ) ) ;
#5165 = CARTESIAN_POINT ( 'NONE',  ( 0.000000000000000000, 0.000000000000000000, 0.000000000000000000 ) ) ;
#5166 = VECTOR ( 'NONE', #21691, 1000.000000000000000 ) ;
#5167 = CC_DESIGN_DATE_AND_TIME_ASSIGNMENT ( #9842, #6271, ( #5355 ) ) ;
#5168 = FACE_OUTER_BOUND ( 'NONE', #6993, .T. ) ;
#5169 = ORIENTED_EDGE ( 'NONE', *, *, #17945, .F. ) ;
#5170 = DIRECTION ( 'NONE',  ( -0.2306359803922031215, -0.9730401042858033422, 0.000000000000000000 ) ) ;
#5171 = EDGE_CURVE ( 'NONE', #21047, #300, #23015, .T. ) ;
#5172 = EDGE_CURVE ( 'NONE', #19198, #12333, #6067, .T. ) ;
#5173 = DESIGN_CONTEXT ( 'detailed design', #6565, 'design' ) ;
#5174 = DIRECTION ( 'NONE',  ( 0.000000000000000000, 0.000000000000000000, 1.000000000000000000 ) ) ;
#5175 = APPROVAL ( #11695, 'UNSPECIFIED' ) ;
#5176 = EDGE_LOOP ( 'NONE', ( #13243, #16470 ) ) ;
#5177 = CARTESIAN_POINT ( 'NONE',  ( 58.73439644601039333, 17.65016624305030035, 13.00000000000000000 ) ) ;
#5178 = CARTESIAN_POINT ( 'NONE',  ( -2.499999999999973799, 4.120723506284736299E-15, 5.000000000000000000 ) ) ;
#5179 = ORIENTED_EDGE ( 'NONE', *, *, #4857, .F. ) ;
#5180 = PERSON_AND_ORGANIZATION ( #22372, #20517 ) ;
#5181 = CARTESIAN_POINT ( 'NONE',  ( -70.63306599754589854, 6.130251853413639651, -5.500000000000079048 ) ) ;
#5182 = ORIENTED_EDGE ( 'NONE', *, *, #18231, .F. ) ;
#5183 = ORIENTED_EDGE ( 'NONE', *, *, #96, .F. ) ;
#5184 = APPROVAL_ROLE ( '' ) ;
#5185 = DIRECTION ( 'NONE',  ( -0.2306359803922028995, -0.9730401042858035643, 3.648592655857288816E-32 ) ) ;
#5186 = ORIENTED_EDGE ( 'NONE', *, *, #20712, .F. ) ;
#5187 = CIRCLE ( 'NONE', #4812, 0.4000000000000010214 ) ;
#5188 = AXIS2_PLACEMENT_3D ( 'NONE', #15838, #3132, #17395 ) ;
#5189 = DIRECTION ( 'NONE',  ( 0.2306359803922083396, 0.9730401042858023430, 8.673617379884037996E-14 ) ) ;
#5190 = CIRCLE ( 'NONE', #18472, 4.250000000000000000 ) ;
#5191 = PERSON_AND_ORGANIZATION_ROLE ( 'creator' ) ;
#5192 = EDGE_CURVE ( 'NONE', #13418, #21387, #6443, .T. ) ;
#5193 = COORDINATED_UNIVERSAL_TIME_OFFSET ( 0, 0, .AHEAD. ) ;
#5194 = LINE ( 'NONE', #12688, #21822 ) ;
#5195 = EDGE_CURVE ( 'NONE', #4561, #21838, #3035, .T. ) ;
#5196 = AXIS2_PLACEMENT_3D ( 'NONE', #20799, #20333, #22334 ) ;
#5197 = CARTESIAN_POINT ( 'NONE',  ( 34.89491389100820129, 23.30074776265920278, 8.749999999999998224 ) ) ;
#5198 = VERTEX_POINT ( 'NONE', #21125 ) ;
#5199 = EDGE_CURVE ( 'NONE', #9773, #6033, #13779, .T. ) ;
#5200 = VECTOR ( 'NONE', #19305, 1000.000000000000114 ) ;
#5201 = EDGE_CURVE ( 'NONE', #9993, #577, #17071, .T. ) ;
#5202 = ORIENTED_EDGE ( 'NONE', *, *, #2871, .T. ) ;
#5203 = CARTESIAN_POINT ( 'NONE',  ( 0.03403376487640599746, -6.499910899608420500, 8.873528816395729098E-14 ) ) ;
#5204 = CARTESIAN_POINT ( 'NONE',  ( -67.24235627552209849, 7.607684554713948444, 2.499999999999999556 ) ) ;
#5205 = ORIENTED_EDGE ( 'NONE', *, *, #15038, .T. ) ;
#5206 = CARTESIAN_POINT ( 'NONE',  ( -12.59661859123020022, -1.225550774622840233, -5.499999999997189803 ) ) ;
#5207 = DIRECTION ( 'NONE',  ( -2.982858504577330093E-17, 2.441916418604790135E-15, 1.000000000000000000 ) ) ;
#5208 = CIRCLE ( 'NONE', #3308, 7.999999999999998224 ) ;
#5209 = ORIENTED_EDGE ( 'NONE', *, *, #18986, .F. ) ;
#5210 =( REPRESENTATION_RELATIONSHIP ('NONE','NONE', #18771, #22961 ) REPRESENTATION_RELATIONSHIP_WITH_TRANSFORMATION ( #10152 )SHAPE_REPRESENTATION_RELATIONSHIP( ) );
#5211 = VERTEX_POINT ( 'NONE', #3202 ) ;
#5212 = APPROVAL_DATE_TIME ( #19819, #1680 ) ;
#5213 = ORIENTED_EDGE ( 'NONE', *, *, #10290, .F. ) ;
#5214 = EDGE_LOOP ( 'NONE', ( #23074, #15099, #17, #17124 ) ) ;
#5215 = DIRECTION ( 'NONE',  ( 1.138590270679730064E-14, 2.220446049251235259E-15, 1.000000000000000000 ) ) ;
#5216 = COORDINATED_UNIVERSAL_TIME_OFFSET ( 0, 0, .AHEAD. ) ;
#5217 = VECTOR ( 'NONE', #1597, 1000.000000000000000 ) ;
#5218 = AXIS2_PLACEMENT_3D ( 'NONE', #18219, #18351, #15001 ) ;
#5219 = CARTESIAN_POINT ( 'NONE',  ( -13.66074082773489984, 1.277408929928580017, 5.000000000000000000 ) ) ;
#5220 = PERSON_AND_ORGANIZATION ( #20433, #16819 ) ;
#5221 = VECTOR ( 'NONE', #2066, 1000.000000000000227 ) ;
#5222 = EDGE_CURVE ( 'NONE', #10345, #21109, #18214, .T. ) ;
#5223 = EDGE_CURVE ( 'NONE', #16864, #8907, #9884, .T. ) ;
#5224 = FACE_BOUND ( 'NONE', #10101, .T. ) ;
#5225 = AXIS2_PLACEMENT_3D ( 'NONE', #3290, #16230, #9102 ) ;
#5226 = APPROVAL_ROLE ( '' ) ;
#5227 = ORIENTED_EDGE ( 'NONE', *, *, #16658, .T. ) ;
#5228 = VECTOR ( 'NONE', #12942, 999.9999999999998863 ) ;
#5229 = CARTESIAN_POINT ( 'NONE',  ( -1.150383022719682513, 15.76081433601112280, -7.583947952205592060E-15 ) ) ;
#5230 = CARTESIAN_POINT ( 'NONE',  ( 45.07211867146970263, 28.08243186520990164, 13.00000000000000000 ) ) ;
#5231 = ORIENTED_EDGE ( 'NONE', *, *, #17043, .F. ) ;
#5232 = VECTOR ( 'NONE', #16909, 999.9999999999998863 ) ;
#5233 = LINE ( 'NONE', #8923, #21512 ) ;
#5234 = AXIS2_PLACEMENT_3D ( 'NONE', #8009, #7539, #11479 ) ;
#5235 = DIRECTION ( 'NONE',  ( 2.270069654138865127E-15, 1.000000000000000000, -4.574083617919690056E-30 ) ) ;
#5236 = ORIENTED_EDGE ( 'NONE', *, *, #5711, .T. ) ;
#5237 = VERTEX_POINT ( 'NONE', #17235 ) ;
#5238 = CARTESIAN_POINT ( 'NONE',  ( 2.499999999999970246, -28.60000000000000142, 19.00000000000000000 ) ) ;
#5239 = APPROVAL_DATE_TIME ( #14380, #1247 ) ;
#5240 = EDGE_CURVE ( 'NONE', #7095, #22844, #15320, .T. ) ;
#5241 = ORIENTED_EDGE ( 'NONE', *, *, #16937, .F. ) ;
#5242 = VERTEX_POINT ( 'NONE', #10469 ) ;
#5243 = CARTESIAN_POINT ( 'NONE',  ( -4.620515280316187769E-46, 7.545869370336972286E-30, -21.50000000000000000 ) ) ;
#5244 = DIRECTION ( 'NONE',  ( -3.099353312215988811E-62, 0.000000000000000000, 1.000000000000000000 ) ) ;
#5245 = CALENDAR_DATE ( 2026, 31, 10 ) ;
#5246 = CARTESIAN_POINT ( 'NONE',  ( 36.57467860885130051, 21.71590586959130320, -15.00000000000049916 ) ) ;
#5247 = CARTESIAN_POINT ( 'NONE',  ( -60.24907127679855279, 13.37794642375635590, -5.845314026106529258E-15 ) ) ;
#5248 = AXIS2_PLACEMENT_3D ( 'NONE', #8622, #6841, #6618 ) ;
#5249 = VECTOR ( 'NONE', #11332, 1000.000000000000000 ) ;
#5250 = DIRECTION ( 'NONE',  ( 0.000000000000000000, 0.000000000000000000, 1.000000000000000000 ) ) ;
#5251 = LINE ( 'NONE', #21408, #18540 ) ;
#5252 = DATE_AND_TIME ( #23174, #6122 ) ;
#5253 = LINE ( 'NONE', #18084, #9115 ) ;
#5254 = CARTESIAN_POINT ( 'NONE',  ( -22.49941224781415627, 22.89788185598131420, -5.000000000000000000 ) ) ;
#5255 = CYLINDRICAL_SURFACE ( 'NONE', #235, 49.22658835543908395 ) ;
#5256 = CARTESIAN_POINT ( 'NONE',  ( 40.45939906362549721, 8.621629779493760637, 3.888892445930440142E-14 ) ) ;
#5257 = DIRECTION ( 'NONE',  ( -0.9730401042858035643, 0.2306359803922028717, 5.959266323858677443E-17 ) ) ;
#5258 = ORIENTED_EDGE ( 'NONE', *, *, #18536, .T. ) ;
#5259 = DIRECTION ( 'NONE',  ( 1.000000000000000000, -6.281952996264290168E-17, 3.503246160812045303E-47 ) ) ;
#5260 = ADVANCED_FACE ( 'NONE', ( #4508, #1295, #17340 ), #11904, .F. ) ;
#5261 = EDGE_CURVE ( 'NONE', #8547, #11347, #14042, .T. ) ;
#5262 = CLOSED_SHELL ( 'NONE', ( #6568, #1932, #19282, #11447, #3447, #1088, #19566, #23104, #4357, #19148, #11998, #21855, #8561, #1001, #15798, #16064, #1082, #15892, #6164, #6863, #7247 ) ) ;
#5263 = EDGE_LOOP ( 'NONE', ( #12585, #13550 ) ) ;
#5264 = CARTESIAN_POINT ( 'NONE',  ( 39.37089837072289811, 22.23982225285509884, 13.00000000000000000 ) ) ;
#5265 = DIRECTION ( 'NONE',  ( -1.000000000000000000, 2.270069654138870255E-15, -3.099353312215989243E-62 ) ) ;
#5266 = VERTEX_POINT ( 'NONE', #15789 ) ;
#5267 = CARTESIAN_POINT ( 'NONE',  ( -20.00000001665708282, -17.50000000000000000, -7.999999999995464073 ) ) ;
#5268 = ORIENTED_EDGE ( 'NONE', *, *, #18337, .F. ) ;
#5269 = CARTESIAN_POINT ( 'NONE',  ( -27.00000000000000000, -20.00000000000000000, -2.500000000000000000 ) ) ;
#5270 = DATE_AND_TIME ( #1467, #13406 ) ;
#5271 = CIRCLE ( 'NONE', #19687, 2.500000000000000444 ) ;
#5272 = CARTESIAN_POINT ( 'NONE',  ( 113.2956221386590130, -28.78551670568849730, 3.100000000000000089 ) ) ;
#5273 = EDGE_CURVE ( 'NONE', #20204, #9841, #10233, .T. ) ;
#5274 = EDGE_CURVE ( 'NONE', #17960, #11172, #16670, .T. ) ;
#5275 = FACE_OUTER_BOUND ( 'NONE', #12103, .T. ) ;
#5276 = CYLINDRICAL_SURFACE ( 'NONE', #22276, 2.499999999999998668 ) ;
#5277 = DIRECTION ( 'NONE',  ( 0.000000000000000000, 0.000000000000000000, 1.000000000000000000 ) ) ;
#5278 = LINE ( 'NONE', #14424, #21763 ) ;
#5279 = LINE ( 'NONE', #2069, #5217 ) ;
#5280 = CYLINDRICAL_SURFACE ( 'NONE', #15390, 2.499999999999998224 ) ;
#5281 = CARTESIAN_POINT ( 'NONE',  ( -60.02994014102380049, 8.478793778983318319, -5.000000000000000000 ) ) ;
#5282 = ORIENTED_EDGE ( 'NONE', *, *, #17214, .T. ) ;
#5283 = CC_DESIGN_SECURITY_CLASSIFICATION ( #3753, ( #23480 ) ) ;
#5284 = DIRECTION ( 'NONE',  ( 3.794988516547419626E-16, 3.848888668432490244E-16, -1.000000000000000000 ) ) ;
#5285 = AXIS2_PLACEMENT_3D ( 'NONE', #149, #5265, #10764 ) ;
#5286 = DIRECTION ( 'NONE',  ( 0.9730401042858036753, -0.2306359803922031493, 2.804983810440361760E-16 ) ) ;
#5287 = VERTEX_POINT ( 'NONE', #5417 ) ;
#5288 = EDGE_CURVE ( 'NONE', #6720, #13613, #20818, .T. ) ;
#5289 = CONTEXT_DEPENDENT_SHAPE_REPRESENTATION ( #11394, #7994 ) ;
#5290 = CARTESIAN_POINT ( 'NONE',  ( -32.65691263631629226, 9.274125246214069307, 2.500000000000000000 ) ) ;
#5291 = VERTEX_POINT ( 'NONE', #20021 ) ;
#5293 = COORDINATED_UNIVERSAL_TIME_OFFSET ( 0, 0, .AHEAD. ) ;
#5292 = APPROVAL ( #20522, 'UNKNOWN' ) ;
#5294 = CARTESIAN_POINT ( 'NONE',  ( 52.05497947389309843, 22.85602965967900246, 3.416161896595049310E-14 ) ) ;
#5295 = ORIENTED_EDGE ( 'NONE', *, *, #313, .F. ) ;
#5296 = PRODUCT_RELATED_PRODUCT_CATEGORY ( 'detail', '', ( #19920 ) ) ;
#5297 = DIRECTION ( 'NONE',  ( -0.2306359803922080343, -0.9730401042858022320, 2.974717104243940401E-15 ) ) ;
#5298 = PERSON_AND_ORGANIZATION ( #11966, #8758 ) ;
#5299 = EDGE_CURVE ( 'NONE', #3862, #2850, #11255, .T. ) ;
#5300 = EDGE_CURVE ( 'NONE', #20016, #21792, #9219, .T. ) ;
#5301 = PRODUCT_DEFINITION_SHAPE ( 'NONE', 'NONE',  #6763 ) ;
#5302 = APPROVAL_DATE_TIME ( #3532, #21957 ) ;
#5303 = VECTOR ( 'NONE', #7908, 1000.000000000000114 ) ;
#5304 = CARTESIAN_POINT ( 'NONE',  ( -31.64684134471649912, 7.334398819369059908, -3.750000000000000000 ) ) ;
#5305 = ADVANCED_FACE ( 'NONE', ( #13135 ), #5530, .F. ) ;
#5306 = AXIS2_PLACEMENT_3D ( 'NONE', #10607, #5352, #7264 ) ;
#5307 = CYLINDRICAL_SURFACE ( 'NONE', #11173, 2.500000000000000444 ) ;
#5308 = ORIENTED_EDGE ( 'NONE', *, *, #11292, .F. ) ;
#5310 = AXIS2_PLACEMENT_3D ( 'NONE', #10130, #1185, #15805 ) ;
#5309 = LINE ( 'NONE', #11030, #3366 ) ;
#5311 = EDGE_LOOP ( 'NONE', ( #8292, #1196 ) ) ;
#5312 = CYLINDRICAL_SURFACE ( 'NONE', #16169, 5.000000000000000888 ) ;
#5313 = PLANE ( 'NONE',  #16355 ) ;
#5314 = DIRECTION ( 'NONE',  ( -0.9730401042858024541, 0.2306359803922080898, 5.959266323858942451E-17 ) ) ;
#5315 = ORIENTED_EDGE ( 'NONE', *, *, #13319, .T. ) ;
#5316 = EDGE_CURVE ( 'NONE', #5040, #6499, #15897, .T. ) ;
#5317 = CC_DESIGN_SECURITY_CLASSIFICATION ( #6843, ( #3780 ) ) ;
#5318 = DIRECTION ( 'NONE',  ( -0.2306359803922085339, -0.9730401042858022320, 0.000000000000000000 ) ) ;
#5319 = CARTESIAN_POINT ( 'NONE',  ( 122.7747609327790030, 11.20643158045800014, -9.133960000000000079 ) ) ;
#5320 = ORIENTED_EDGE ( 'NONE', *, *, #22912, .F. ) ;
#5321 = ORIENTED_EDGE ( 'NONE', *, *, #21465, .F. ) ;
#5322 = VECTOR ( 'NONE', #7206, 1000.000000000000114 ) ;
#5323 = MECHANICAL_CONTEXT ( 'NONE', #14734, 'mechanical' ) ;
#5324 = ORIENTED_EDGE ( 'NONE', *, *, #498, .T. ) ;
#5325 = ORIENTED_EDGE ( 'NONE', *, *, #1097, .T. ) ;
#5326 = CARTESIAN_POINT ( 'NONE',  ( -57.14322836594880073, 8.493908704608589488, 2.318032717970499742E-15 ) ) ;
#5327 = APPROVAL_DATE_TIME ( #7369, #4013 ) ;
#5328 = AXIS2_PLACEMENT_3D ( 'NONE', #11928, #15565, #22802 ) ;
#5329 = EDGE_CURVE ( 'NONE', #11214, #2666, #8668, .T. ) ;
#5330 = EDGE_CURVE ( 'NONE', #1337, #547, #21909, .T. ) ;
#5331 = LINE ( 'NONE', #7472, #19942 ) ;
#5332 = DATE_AND_TIME ( #15239, #21952 ) ;
#5333 = APPLICATION_CONTEXT ( 'configuration controlled 3d designs of mechanical parts and assemblies' ) ;
#5334 = APPROVAL_PERSON_ORGANIZATION ( #3930, #4742, #21847 ) ;
#5335 = APPROVAL_PERSON_ORGANIZATION ( #4254, #1243, #2708 ) ;
#5336 = CARTESIAN_POINT ( 'NONE',  ( 51.09971998237313784, 11.23812949209873935, 3.823728413317720161E-14 ) ) ;
#5337 = CIRCLE ( 'NONE', #10358, 12.49999999999999467 ) ;
#5338 = CALENDAR_DATE ( 2026, 31, 10 ) ;
#5339 = ORIENTED_EDGE ( 'NONE', *, *, #16091, .T. ) ;
#5340 = ORIENTED_EDGE ( 'NONE', *, *, #22749, .T. ) ;
#5341 = PLANE ( 'NONE',  #3062 ) ;
#5342 = DIRECTION ( 'NONE',  ( 2.471194949999149731E-15, 1.016744709403700171E-14, 1.000000000000000000 ) ) ;
#5343 = AXIS2_PLACEMENT_3D ( 'NONE', #19314, #4713, #8395 ) ;
#5344 = ORIENTED_EDGE ( 'NONE', *, *, #14514, .T. ) ;
#5345 = EDGE_CURVE ( 'NONE', #22438, #2098, #6461, .T. ) ;
#5346 = FACE_OUTER_BOUND ( 'NONE', #18860, .T. ) ;
#5347 = DIRECTION ( 'NONE',  ( 1.138590270679734009E-14, 2.220446049251240387E-15, 1.000000000000000000 ) ) ;
#5348 = SHAPE_REPRESENTATION ( 'Fixed base', ( #12739 ), #1341 ) ;
#5349 = CARTESIAN_POINT ( 'NONE',  ( -1.262685242559879909E-14, -17.30000000000000071, 2.500000000000000000 ) ) ;
#5350 = ORIENTED_EDGE ( 'NONE', *, *, #1526, .F. ) ;
#5351 = EDGE_LOOP ( 'NONE', ( #3583, #17772, #16976, #13733 ) ) ;
#5352 = DIRECTION ( 'NONE',  ( 1.138590270679730064E-14, 2.220446049251230526E-15, 1.000000000000000000 ) ) ;
#5353 = ORIENTED_EDGE ( 'NONE', *, *, #19159, .F. ) ;
#5354 = CALENDAR_DATE ( 2026, 31, 10 ) ;
#5355 = SECURITY_CLASSIFICATION ( '', '', #6030 ) ;
#5356 = EDGE_LOOP ( 'NONE', ( #12461, #22910, #18015, #1741 ) ) ;
#5357 = ORIENTED_EDGE ( 'NONE', *, *, #19814, .F. ) ;
#5358 = FACE_OUTER_BOUND ( 'NONE', #12719, .T. ) ;
#5359 = DIRECTION ( 'NONE',  ( 0.2306359803922076457, 0.9730401042858023430, 0.000000000000000000 ) ) ;
#5360 = APPROVAL_PERSON_ORGANIZATION ( #15941, #11056, #19873 ) ;
#5361 = CARTESIAN_POINT ( 'NONE',  ( 26.11627841292220253, -8.532812502301570845, 16.00000000000000000 ) ) ;
#5362 = APPROVAL_ROLE ( '' ) ;
#5363 = EDGE_CURVE ( 'NONE', #12123, #23452, #14437, .T. ) ;
#5364 = CARTESIAN_POINT ( 'NONE',  ( -2.500000000000000000, -17.30000000000000071, -5.000000000000000000 ) ) ;
#5365 = ADVANCED_FACE ( 'NONE', ( #12783 ), #20262, .F. ) ;
#5366 = LINE ( 'NONE', #9523, #18988 ) ;
#5367 = LOCAL_TIME ( 14, 11, 27.00000000000000000, #13175 ) ;
#5368 = CARTESIAN_POINT ( 'NONE',  ( 0.000000000000000000, 0.000000000000000000, 0.000000000000000000 ) ) ;
#5369 = DIRECTION ( 'NONE',  ( 0.000000000000000000, -2.098117411679737831E-16, -1.000000000000000000 ) ) ;
#5370 = CALENDAR_DATE ( 2026, 31, 10 ) ;
#5371 = LOCAL_TIME ( 14, 11, 27.00000000000000000, #8407 ) ;
#5372 = DIRECTION ( 'NONE',  ( -6.662111338785949120E-09, 1.000000000000000000, -1.982541115402066096E-15 ) ) ;
#5373 = CONICAL_SURFACE ( 'NONE', #5743, 1.154700538379250796, 1.047197551196598297 ) ;
#5374 = DIRECTION ( 'NONE',  ( -0.9997648975362221080, -0.02168293463503390486, 0.000000000000000000 ) ) ;
#5375 = DIRECTION ( 'NONE',  ( -8.911056267098788616E-18, -1.998401444326210262E-15, -1.000000000000000000 ) ) ;
#5376 = PLANE ( 'NONE',  #18877 ) ;
#5377 = DIRECTION ( 'NONE',  ( 0.1630842657209339019, 0.6880432561069519393, -0.7071067811865526798 ) ) ;
#5378 = ORIENTED_EDGE ( 'NONE', *, *, #23018, .T. ) ;
#5379 = APPROVAL_PERSON_ORGANIZATION ( #16117, #4416, #23462 ) ;
#5380 = CARTESIAN_POINT ( 'NONE',  ( 34.99546711040250102, 11.77144200483400915, 8.817835639223813970 ) ) ;
#5381 = CC_DESIGN_DATE_AND_TIME_ASSIGNMENT ( #22948, #19055, ( #9917 ) ) ;
#5382 = ORIENTED_EDGE ( 'NONE', *, *, #517, .T. ) ;
#5383 = CARTESIAN_POINT ( 'NONE',  ( 27.94580623989299895, -3.849224340072050055, 13.50000000000019895 ) ) ;
#5384 = DIRECTION ( 'NONE',  ( -3.210834492181040124E-17, 2.441916418604790135E-15, 1.000000000000000000 ) ) ;
#5385 = ORIENTED_EDGE ( 'NONE', *, *, #6086, .F. ) ;
#5386 = CARTESIAN_POINT ( 'NONE',  ( 31.11077410011089839, -1.335996977273280262, -11.00000000000039968 ) ) ;
#5387 = EDGE_LOOP ( 'NONE', ( #15085, #6435, #1513, #16733 ) ) ;
#5388 = LOCAL_TIME ( 14, 11, 27.00000000000000000, #14971 ) ;
#5389 = DIRECTION ( 'NONE',  ( -2.102818713247520211E-14, -6.140746379865968924E-31, -1.000000000000000000 ) ) ;
#5390 = APPROVAL_DATE_TIME ( #18000, #23283 ) ;
#5391 = AXIS2_PLACEMENT_3D ( 'NONE', #16415, #10872, #16187 ) ;
#5393 = DIRECTION ( 'NONE',  ( 6.009176021521548497E-19, -0.9999588795606765279, 0.009068582455730085992 ) ) ;
#5392 = PERSON ( 'NAUO-PER33', 'UNSPECIFIED', 'UNSPECIFIED', ('UNSPECIFIED'), ('UNSPECIFIED'), ('UNSPECIFIED') ) ;
#5394 = AXIS2_PLACEMENT_3D ( 'NONE', #18396, #4011, #9127 ) ;
#5395 = VECTOR ( 'NONE', #7700, 1000.000000000000000 ) ;
#5396 = AXIS2_PLACEMENT_3D ( 'NONE', #13362, #22366, #22598 ) ;
#5397 = CC_DESIGN_APPROVAL ( #22683, ( #22065 ) ) ;
#5398 = DIRECTION ( 'NONE',  ( 0.000000000000000000, 0.000000000000000000, 1.000000000000000000 ) ) ;
#5399 = AXIS2_PLACEMENT_3D ( 'NONE', #23422, #14288, #5725 ) ;
#5400 = EDGE_CURVE ( 'NONE', #17785, #8770, #11408, .T. ) ;
#5401 = DIRECTION ( 'NONE',  ( -0.7070970883417637687, -0.003702385528188433840, 0.7071067811865477948 ) ) ;
#5402 = COORDINATED_UNIVERSAL_TIME_OFFSET ( 0, 0, .AHEAD. ) ;
#5403 = CYLINDRICAL_SURFACE ( 'NONE', #23285, 3.499999999999999556 ) ;
#5404 = CARTESIAN_POINT ( 'NONE',  ( -20.00000000397430000, 22.95208919257349933, -6.749999999995570654 ) ) ;
#5405 = DIRECTION ( 'NONE',  ( -0.9730401042858035643, 0.2306359803922028717, 5.958148513035547083E-17 ) ) ;
#5406 = LOCAL_TIME ( 14, 11, 27.00000000000000000, #5216 ) ;
#5407 = CARTESIAN_POINT ( 'NONE',  ( -57.35420414587308358, -25.07745730012768703, -5.538319619822460249E-15 ) ) ;
#5408 = ORIENTED_EDGE ( 'NONE', *, *, #15063, .F. ) ;
#5409 = CARTESIAN_POINT ( 'NONE',  ( -16.50082286259691955, 23.02797946379192950, -2.500000000000059952 ) ) ;
#5410 = CIRCLE ( 'NONE', #17541, 2.699999999999998845 ) ;
#5411 = FACE_OUTER_BOUND ( 'NONE', #14757, .T. ) ;
#5412 = AXIS2_PLACEMENT_3D ( 'NONE', #14668, #20261, #18481 ) ;
#5413 = ORIENTED_EDGE ( 'NONE', *, *, #4879, .T. ) ;
#5414 = ADVANCED_BREP_SHAPE_REPRESENTATION ( '', ( #9367, #12739 ), #1734 ) ;
#5415 = VECTOR ( 'NONE', #8726, 1000.000000000000114 ) ;
#5416 = DIRECTION ( 'NONE',  ( -0.1997366180463769070, -0.8426774492125652660, 0.5000000000000002220 ) ) ;
#5417 = CARTESIAN_POINT ( 'NONE',  ( -16.50000000000000000, -20.00000000000000711, 5.000000000000000000 ) ) ;
#5418 = VERTEX_POINT ( 'NONE', #18482 ) ;
#5419 = APPROVAL_ROLE ( '' ) ;
#5420 = AXIS2_PLACEMENT_3D ( 'NONE', #21067, #1102, #15606 ) ;
#5421 = FACE_BOUND ( 'NONE', #11269, .T. ) ;
#5422 = ORIENTED_EDGE ( 'NONE', *, *, #17971, .T. ) ;
#5423 = LINE ( 'NONE', #61, #18141 ) ;
#5424 = AXIS2_PLACEMENT_3D ( 'NONE', #6839, #20844, #19308 ) ;
#5425 = APPROVAL_ROLE ( '' ) ;
#5426 = VECTOR ( 'NONE', #7588, 999.9999999999998863 ) ;
#5427 = PRODUCT_DEFINITION_FORMATION_WITH_SPECIFIED_SOURCE ( 'ANY', '', #11806, .NOT_KNOWN. ) ;
#5428 = CARTESIAN_POINT ( 'NONE',  ( -26.00000000000000000, -20.00000000055539928, 6.750000000004630074 ) ) ;
#5429 = VECTOR ( 'NONE', #6406, 999.9999999999998863 ) ;
#5430 = VECTOR ( 'NONE', #6923, 999.9999999999998863 ) ;
#5431 = EDGE_CURVE ( 'NONE', #16449, #19011, #11014, .T. ) ;
#5432 = AXIS2_PLACEMENT_3D ( 'NONE', #5019, #19620, #3232 ) ;
#5433 = CARTESIAN_POINT ( 'NONE',  ( -62.93660361792420588, 12.27413839645710070, 3.322570288448809768E-15 ) ) ;
#5434 = ORIENTED_EDGE ( 'NONE', *, *, #17059, .F. ) ;
#5435 = DIRECTION ( 'NONE',  ( 0.9730401042858035643, -0.2306359803922028717, -8.741838862554660940E-17 ) ) ;
#5436 = APPROVAL ( #7676, 'UNKNOWN' ) ;
#5437 = ORIENTED_EDGE ( 'NONE', *, *, #15135, .F. ) ;
#5438 = AXIS2_PLACEMENT_3D ( 'NONE', #9077, #23323, #11120 ) ;
#5439 = FACE_OUTER_BOUND ( 'NONE', #3247, .T. ) ;
#5440 = DIRECTION ( 'NONE',  ( 0.2306359803922085339, 0.9730401042858022320, 0.000000000000000000 ) ) ;
#5441 = CARTESIAN_POINT ( 'NONE',  ( 28.67817383939640052, -0.7594070262927730131, -15.00000000000039968 ) ) ;
#5442 = ORIENTED_EDGE ( 'NONE', *, *, #19017, .F. ) ;
#5443 = EDGE_CURVE ( 'NONE', #5968, #10008, #23465, .T. ) ;
#5444 = EDGE_CURVE ( 'NONE', #20801, #16051, #322, .T. ) ;
#5445 = SECURITY_CLASSIFICATION ( '', '', #3260 ) ;
#5446 = DIRECTION ( 'NONE',  ( -3.210834492181045054E-17, 2.441916418604795262E-15, 1.000000000000000000 ) ) ;
#5447 = CARTESIAN_POINT ( 'NONE',  ( 33.27705887009690144, -3.036156860537205127, -17.25000000000040146 ) ) ;
#5448 = ORIENTED_EDGE ( 'NONE', *, *, #3722, .F. ) ;
#5449 = CALENDAR_DATE ( 2026, 31, 10 ) ;
#5450 = EDGE_LOOP ( 'NONE', ( #8169, #6274 ) ) ;
#5451 = VECTOR ( 'NONE', #15286, 1000.000000000000000 ) ;
#5452 = ORIENTED_EDGE ( 'NONE', *, *, #9286, .T. ) ;
#5453 = PLANE ( 'NONE',  #1616 ) ;
#5454 = EDGE_CURVE ( 'NONE', #18495, #20452, #2197, .T. ) ;
#5455 = COORDINATED_UNIVERSAL_TIME_OFFSET ( 0, 0, .AHEAD. ) ;
#5456 = APPROVAL_STATUS ( 'not_yet_approved' ) ;
#5457 = PLANE ( 'NONE',  #16876 ) ;
#5458 = ADVANCED_FACE ( 'NONE', ( #5885 ), #14913, .T. ) ;
#5459 = CIRCLE ( 'NONE', #1652, 3.499999999999996891 ) ;
#5460 = SHAPE_REPRESENTATION_RELATIONSHIP ( 'NONE' , 'NONE' ,  #2509, #7943 ) ;
#5461 = LINE ( 'NONE', #14602, #19084 ) ;
#5462 = VECTOR ( 'NONE', #17829, 1000.000000000000114 ) ;
#5463 = APPROVAL ( #2256, 'UNSPECIFIED' ) ;
#5464 = DATE_AND_TIME ( #21487, #2716 ) ;
#5465 = APPROVAL ( #15926, 'UNSPECIFIED' ) ;
#5466 = ORIENTED_EDGE ( 'NONE', *, *, #8985, .T. ) ;
#5467 = LINE ( 'NONE', #18056, #12422 ) ;
#5468 = ORIENTED_EDGE ( 'NONE', *, *, #5300, .F. ) ;
#5469 = EDGE_CURVE ( 'NONE', #16018, #15497, #378, .T. ) ;
#5470 = EDGE_CURVE ( 'NONE', #14320, #18371, #7307, .T. ) ;
#5471 = DIRECTION ( 'NONE',  ( 2.982858504489129897E-17, -2.441916418604790135E-15, -1.000000000000000000 ) ) ;
#5472 = DIRECTION ( 'NONE',  ( 0.000000000000000000, 0.000000000000000000, 1.000000000000000000 ) ) ;
#5473 = DIRECTION ( 'NONE',  ( -0.9730401042858035643, 0.2306359803922028717, -2.804983810440358308E-16 ) ) ;
#5474 = ORIENTED_EDGE ( 'NONE', *, *, #11343, .F. ) ;
#5475 = ORIENTED_EDGE ( 'NONE', *, *, #12471, .F. ) ;
#5476 = CARTESIAN_POINT ( 'NONE',  ( 49.97703550743810297, 19.72589006658010291, 15.50000000000000000 ) ) ;
#5477 = ORIENTED_EDGE ( 'NONE', *, *, #530, .T. ) ;
#5478 = COORDINATED_UNIVERSAL_TIME_OFFSET ( 0, 0, .AHEAD. ) ;
#5479 = EDGE_LOOP ( 'NONE', ( #16754, #20151, #11497, #19701 ) ) ;
#5480 = ORIENTED_EDGE ( 'NONE', *, *, #17700, .F. ) ;
#5481 = CARTESIAN_POINT ( 'NONE',  ( -19.49999999982519938, -0.1021026942257659970, 5.000000000000000000 ) ) ;
#5482 = CARTESIAN_POINT ( 'NONE',  ( 30.31182762792540331, -4.706706774123410320, 13.00000000000019895 ) ) ;
#5483 = SHAPE_DEFINITION_REPRESENTATION ( #6421, #488 ) ;
#5484 = APPLICATION_CONTEXT ( 'configuration controlled 3d designs of mechanical parts and assemblies' ) ;
#5485 = DIRECTION ( 'NONE',  ( -0.9730401042858035643, 0.2306359803922028717, 5.958148513035547083E-17 ) ) ;
#5486 = CARTESIAN_POINT ( 'NONE',  ( -26.68810977484059777, -6.639828994528159889, 2.501000000000090484 ) ) ;
#5487 = EDGE_CURVE ( 'NONE', #17995, #15230, #7555, .T. ) ;
#5488 = DIRECTION ( 'NONE',  ( 0.000000000000000000, 0.000000000000000000, 1.000000000000000000 ) ) ;
#5489 = EDGE_LOOP ( 'NONE', ( #8438, #20778, #11834, #1227 ) ) ;
#5490 = DIRECTION ( 'NONE',  ( -0.9730401042858022320, 0.2306359803922080343, 5.959266323858941219E-17 ) ) ;
#5491 = CALENDAR_DATE ( 2026, 31, 10 ) ;
#5492 = EDGE_CURVE ( 'NONE', #16244, #4999, #16633, .T. ) ;
#5493 = SHAPE_REPRESENTATION ( '1602p_c_21', ( #12739 ), #10500 ) ;
#5494 = LINE ( 'NONE', #8840, #14416 ) ;
#5495 = DIRECTION ( 'NONE',  ( 0.000000000000000000, 0.000000000000000000, -1.000000000000000000 ) ) ;
#5496 = ADVANCED_FACE ( 'NONE', ( #2317 ), #6038, .T. ) ;
#5497 = CIRCLE ( 'NONE', #14600, 15.25000000000000000 ) ;
#5498 = CARTESIAN_POINT ( 'NONE',  ( 33.95095283150600807, -0.6266201978619101443, -13.00000000000039968 ) ) ;
#5499 = LINE ( 'NONE', #9298, #23386 ) ;
#5500 = ADVANCED_FACE ( 'NONE', ( #4564 ), #18945, .T. ) ;
#5501 = DIRECTION ( 'NONE',  ( -4.625706045737360025E-15, 0.000000000000000000, 1.000000000000000000 ) ) ;
#5502 = VERTEX_POINT ( 'NONE', #6465 ) ;
#5503 = CARTESIAN_POINT ( 'NONE',  ( 33.57591379187338987, 9.308427061869513963, 8.953813951970682083 ) ) ;
#5504 = PRODUCT ( '1602p_c_47', '1602p_c_47', '', ( #9172 ) ) ;
#5505 = ORIENTED_EDGE ( 'NONE', *, *, #5160, .T. ) ;
#5506 = DIRECTION ( 'NONE',  ( -0.2306359803922040930, -0.9730401042858032312, 4.616450158279817280E-15 ) ) ;
#5507 = CARTESIAN_POINT ( 'NONE',  ( -22.75000000397123046, 22.95208919256889857, 8.500000000005087486 ) ) ;
#5508 = VERTEX_POINT ( 'NONE', #22604 ) ;
#5509 = DIRECTION ( 'NONE',  ( 0.9730401042858036753, -0.2306359803922031493, 2.804983810440361760E-16 ) ) ;
#5510 = EDGE_LOOP ( 'NONE', ( #1914, #21959, #4347, #22692 ) ) ;
#5511 = AXIS2_PLACEMENT_3D ( 'NONE', #2231, #22180, #15301 ) ;
#5512 = CARTESIAN_POINT ( 'NONE',  ( -62.82872441665799101, -8.329083101359751495, -7.727128097349530051E-15 ) ) ;
#5513 = SHAPE_DEFINITION_REPRESENTATION ( #6475, #2026 ) ;
#5514 = DIRECTION ( 'NONE',  ( -0.9730401042858035643, 0.2306359803922028717, 5.667427308550587516E-17 ) ) ;
#5515 = DIRECTION ( 'NONE',  ( 0.2306359803922080343, 0.9730401042858022320, 7.611545645953073104E-14 ) ) ;
#5516 = CC_DESIGN_PERSON_AND_ORGANIZATION_ASSIGNMENT ( #8917, #3572, ( #9941 ) ) ;
#5517 = CARTESIAN_POINT ( 'NONE',  ( 35.89100945995100034, 24.25134070964839950, -11.00000000000049916 ) ) ;
#5518 = DIRECTION ( 'NONE',  ( 1.000000000000000000, 0.000000000000000000, 0.000000000000000000 ) ) ;
#5519 = LINE ( 'NONE', #7194, #9656 ) ;
#5520 = APPLICATION_CONTEXT ( 'configuration controlled 3d designs of mechanical parts and assemblies' ) ;
#5521 = CARTESIAN_POINT ( 'NONE',  ( -19.99975861755300244, 22.95209442650120124, 2.499999999999900524 ) ) ;
#5522 = LINE ( 'NONE', #11130, #21826 ) ;
#5523 = FACE_OUTER_BOUND ( 'NONE', #12129, .T. ) ;
#5524 = CARTESIAN_POINT ( 'NONE',  ( -17.50000000397430000, 22.95208920922877738, -6.749999999996137312 ) ) ;
#5525 = FACE_OUTER_BOUND ( 'NONE', #21960, .T. ) ;
#5526 = EDGE_LOOP ( 'NONE', ( #5886, #22770 ) ) ;
#5527 = CIRCLE ( 'NONE', #1348, 3.750000000000001776 ) ;
#5528 = ORIENTED_EDGE ( 'NONE', *, *, #16814, .T. ) ;
#5529 = CARTESIAN_POINT ( 'NONE',  ( 43.81210844073630994, 9.047859270861110303, -21.50000000000000000 ) ) ;
#5530 = CYLINDRICAL_SURFACE ( 'NONE', #11791, 2.066999999999997950 ) ;
#5531 = ORIENTED_EDGE ( 'NONE', *, *, #4901, .T. ) ;
#5532 = CARTESIAN_POINT ( 'NONE',  ( 2.499999999999970246, -30.47499999999999787, 21.50000000000000000 ) ) ;
#5533 = ADVANCED_FACE ( 'NONE', ( #9933 ), #2798, .T. ) ;
#5534 = ORIENTED_EDGE ( 'NONE', *, *, #3979, .T. ) ;
#5535 = LINE ( 'NONE', #12561, #20401 ) ;
#5536 = PERSON_AND_ORGANIZATION ( #11966, #8758 ) ;
#5537 = AXIS2_PLACEMENT_3D ( 'NONE', #16283, #14171, #17736 ) ;
#5538 = APPROVAL_DATE_TIME ( #21565, #14580 ) ;
#5539 = DIRECTION ( 'NONE',  ( -0.9730401042858024541, 0.2306359803922080898, 5.959266323858942451E-17 ) ) ;
#5540 = CIRCLE ( 'NONE', #16917, 4.999999999999998224 ) ;
#5541 = FACE_OUTER_BOUND ( 'NONE', #7399, .T. ) ;
#5542 = ORIENTED_EDGE ( 'NONE', *, *, #1906, .F. ) ;
#5543 = DIRECTION ( 'NONE',  ( 3.210834492181049985E-17, -2.441916418604790135E-15, -1.000000000000000000 ) ) ;
#5544 = VERTEX_POINT ( 'NONE', #8258 ) ;
#5545 = DIRECTION ( 'NONE',  ( 1.138590270679731958E-14, 2.220446049251245514E-15, 1.000000000000000000 ) ) ;
#5546 = DIRECTION ( 'NONE',  ( 0.9730401042858024541, -0.2306359803922080898, -5.959266323858942451E-17 ) ) ;
#5547 = DIRECTION ( 'NONE',  ( -1.000000000000000000, 0.000000000000000000, 1.159535895544890222E-14 ) ) ;
#5548 = ORIENTED_EDGE ( 'NONE', *, *, #12930, .T. ) ;
#5549 = VECTOR ( 'NONE', #2143, 1000.000000000000000 ) ;
#5550 = COORDINATED_UNIVERSAL_TIME_OFFSET ( 0, 0, .AHEAD. ) ;
#5551 = VECTOR ( 'NONE', #20768, 1000.000000000000000 ) ;
#5552 = FACE_OUTER_BOUND ( 'NONE', #22301, .T. ) ;
#5553 = ORIENTED_EDGE ( 'NONE', *, *, #21146, .F. ) ;
#5554 = PERSON_AND_ORGANIZATION_ROLE ( 'classification_officer' ) ;
#5555 = EDGE_CURVE ( 'NONE', #20782, #10416, #5271, .T. ) ;
#5556 = ORIENTED_EDGE ( 'NONE', *, *, #11755, .T. ) ;
#5557 = ORIENTED_EDGE ( 'NONE', *, *, #17513, .T. ) ;
#5558 = DIRECTION ( 'NONE',  ( 0.9730401042858036753, -0.2306359803922031493, 2.804983810440361760E-16 ) ) ;
#5559 = PERSON_AND_ORGANIZATION ( #11966, #8758 ) ;
#5560 = CC_DESIGN_DATE_AND_TIME_ASSIGNMENT ( #1724, #21551, ( #17878 ) ) ;
#5561 = LINE ( 'NONE', #16370, #1737 ) ;
#5562 = DATE_AND_TIME ( #16371, #8327 ) ;
#5563 = FACE_OUTER_BOUND ( 'NONE', #8371, .T. ) ;
#5564 = EDGE_CURVE ( 'NONE', #16530, #19340, #9454, .T. ) ;
#5565 = ADVANCED_FACE ( 'NONE', ( #15492 ), #22722, .T. ) ;
#5566 = CIRCLE ( 'NONE', #19223, 4.000000000000000000 ) ;
#5567 = AXIS2_PLACEMENT_3D ( 'NONE', #14349, #12239, #12117 ) ;
#5568 = AXIS2_PLACEMENT_3D ( 'NONE', #20940, #6818, #3129 ) ;
#5569 = DIRECTION ( 'NONE',  ( -6.662111466122901068E-09, 1.000000000000000000, -2.220445973397092972E-15 ) ) ;
#5570 = COORDINATED_UNIVERSAL_TIME_OFFSET ( 0, 0, .AHEAD. ) ;
#5571 = VERTEX_POINT ( 'NONE', #16920 ) ;
#5572 = CARTESIAN_POINT ( 'NONE',  ( -62.75803838139569280, -21.82899804532949872, -5.536374493610579731E-15 ) ) ;
#5573 = ORIENTED_EDGE ( 'NONE', *, *, #17834, .F. ) ;
#5574 = CARTESIAN_POINT ( 'NONE',  ( 35.59419854219520118, 9.774809681453358934, -10.74538000000049998 ) ) ;
#5575 = CARTESIAN_POINT ( 'NONE',  ( -20.00000000397430000, 22.95208919257349933, -6.749999999995570654 ) ) ;
#5576 = CARTESIAN_POINT ( 'NONE',  ( 122.4288069621910040, 9.746871424029221131, -10.02499999999999858 ) ) ;
#5577 = VECTOR ( 'NONE', #15342, 1000.000000000000000 ) ;
#5578 = ORIENTED_EDGE ( 'NONE', *, *, #5329, .F. ) ;
#5579 = ORIENTED_EDGE ( 'NONE', *, *, #6381, .F. ) ;
#5580 = CARTESIAN_POINT ( 'NONE',  ( 33.72726576586484981, 23.57751093913000062, 12.99999999999979927 ) ) ;
#5581 = ORIENTED_EDGE ( 'NONE', *, *, #6344, .F. ) ;
#5582 = PERSON_AND_ORGANIZATION_ROLE ( 'classification_officer' ) ;
#5583 = AXIS2_PLACEMENT_3D ( 'NONE', #23352, #19926, #18263 ) ;
#5584 = EDGE_CURVE ( 'NONE', #18769, #2719, #9502, .T. ) ;
#5585 = AXIS2_PLACEMENT_3D ( 'NONE', #5159, #12418, #19652 ) ;
#5586 = ORIENTED_EDGE ( 'NONE', *, *, #22048, .T. ) ;
#5587 = ORIENTED_EDGE ( 'NONE', *, *, #21082, .F. ) ;
#5588 = FACE_OUTER_BOUND ( 'NONE', #11782, .T. ) ;
#5589 = CIRCLE ( 'NONE', #8639, 2.749999999999999112 ) ;
#5590 = CARTESIAN_POINT ( 'NONE',  ( 41.08211621068439712, 11.24883806106539907, 19.59999999999999787 ) ) ;
#5591 = APPROVAL_ROLE ( '' ) ;
#5592 = DIRECTION ( 'NONE',  ( 0.9730401042858035643, -0.2306359803922028717, 2.804983810440357815E-16 ) ) ;
#5593 = CC_DESIGN_DATE_AND_TIME_ASSIGNMENT ( #22150, #11375, ( #480 ) ) ;
#5594 = CC_DESIGN_PERSON_AND_ORGANIZATION_ASSIGNMENT ( #14327, #21556, ( #9939 ) ) ;
#5595 = FACE_OUTER_BOUND ( 'NONE', #14048, .T. ) ;
#5596 = ADVANCED_FACE ( 'NONE', ( #6352 ), #20834, .T. ) ;
#5597 = EDGE_CURVE ( 'NONE', #22958, #13304, #20952, .T. ) ;
#5598 = EDGE_CURVE ( 'NONE', #18732, #12382, #11370, .T. ) ;
#5599 = VECTOR ( 'NONE', #18173, 1000.000000000000000 ) ;
#5600 = EDGE_CURVE ( 'NONE', #13305, #5502, #20614, .T. ) ;
#5601 = ORIENTED_EDGE ( 'NONE', *, *, #13690, .F. ) ;
#5602 = CARTESIAN_POINT ( 'NONE',  ( 35.59419854219520118, 9.774809681453469068, 10.99076000000020059 ) ) ;
#5603 = PERSON_AND_ORGANIZATION_ROLE ( 'creator' ) ;
#5604 = CIRCLE ( 'NONE', #18901, 2.499999999999999112 ) ;
#5605 = ORIENTED_EDGE ( 'NONE', *, *, #20170, .T. ) ;
#5606 = CARTESIAN_POINT ( 'NONE',  ( 45.07211867146820339, 28.08243186520840240, -16.00000000000029843 ) ) ;
#5607 = CARTESIAN_POINT ( 'NONE',  ( -14.00000000000000000, -19.99999999944489915, 5.500000000004489742 ) ) ;
#5608 = DIRECTION ( 'NONE',  ( 5.899155740360660338E-30, 4.861311874477930828E-15, 1.000000000000000000 ) ) ;
#5609 = CARTESIAN_POINT ( 'NONE',  ( -18.05391955182270181, 22.49081825942809942, 2.500000000000000000 ) ) ;
#5610 = LINE ( 'NONE', #12856, #18684 ) ;
#5611 = ORIENTED_EDGE ( 'NONE', *, *, #1067, .F. ) ;
#5612 = CARTESIAN_POINT ( 'NONE',  ( 33.51993406171253298, 9.985323737508171149, 8.999975802806215341 ) ) ;
#5613 = ADVANCED_FACE ( 'NONE', ( #4349 ), #6244, .T. ) ;
#5614 = ORIENTED_EDGE ( 'NONE', *, *, #10780, .F. ) ;
#5615 = ORIENTED_EDGE ( 'NONE', *, *, #5872, .T. ) ;
#5616 = CARTESIAN_POINT ( 'NONE',  ( 28.41185834866789861, -1.882976958576060067, 9.720299461620909298 ) ) ;
#5617 = CONICAL_SURFACE ( 'NONE', #2958, 5.386751345948120218, 1.047197551196598297 ) ;
#5618 = ORIENTED_EDGE ( 'NONE', *, *, #21166, .F. ) ;
#5619 = CARTESIAN_POINT ( 'NONE',  ( -66.39991637198862406, -25.34811502593583654, -3.660254037844378860 ) ) ;
#5620 = ORIENTED_EDGE ( 'NONE', *, *, #18439, .T. ) ;
#5621 = CARTESIAN_POINT ( 'NONE',  ( 26.11627841292220253, -8.532812502301538871, 20.00000000000000000 ) ) ;
#5622 = AXIS2_PLACEMENT_3D ( 'NONE', #11710, #9914, #8596 ) ;
#5623 = DATE_AND_TIME ( #11472, #6592 ) ;
#5624 = DIRECTION ( 'NONE',  ( -0.9997651245102240347, -0.02167246670447264822, 0.000000000000000000 ) ) ;
#5625 = EDGE_CURVE ( 'NONE', #17009, #1957, #11615, .T. ) ;
#5626 = EDGE_CURVE ( 'NONE', #8174, #10214, #14800, .T. ) ;
#5627 =( BOUNDED_CURVE ( )  B_SPLINE_CURVE ( 2, ( #18447, #20680, #18683 ),
 .UNSPECIFIED., .F., .F. ) 
 B_SPLINE_CURVE_WITH_KNOTS ( ( 3, 3 ),
 ( 0.000000000000000000, 0.08763271035584535573 ),
 .UNSPECIFIED. ) 
 CURVE ( )  GEOMETRIC_REPRESENTATION_ITEM ( )  RATIONAL_B_SPLINE_CURVE ( ( 1.000000000000000000, 1.077350269189627063, 1.077350269189624843 ) ) 
 REPRESENTATION_ITEM ( '' )  );
#5628 = CARTESIAN_POINT ( 'NONE',  ( 117.1933702072879981, -12.34113894325840022, 18.89999999999999858 ) ) ;
#5629 = CARTESIAN_POINT ( 'NONE',  ( -20.00000000397450250, 22.95208919256889857, -7.999999999995548450 ) ) ;
#5630 = CARTESIAN_POINT ( 'NONE',  ( -0.2749449575869210571, 0.1862909971238174422, 1.887061435271056409 ) ) ;
#5631 = DIRECTION ( 'NONE',  ( -1.000000000000000000, 1.982541115402065307E-15, 0.000000000000000000 ) ) ;
#5632 = CARTESIAN_POINT ( 'NONE',  ( -2.500000000000000000, 0.000000000000000000, -2.500000000000000000 ) ) ;
#5633 = DIRECTION ( 'NONE',  ( 0.000000000000000000, 0.000000000000000000, 1.000000000000000000 ) ) ;
#5634 = CARTESIAN_POINT ( 'NONE',  ( -23.50000000000000000, -19.99999999999999289, 2.500000000000000000 ) ) ;
#5635 = VECTOR ( 'NONE', #3880, 1000.000000000000000 ) ;
#5636 = FACE_OUTER_BOUND ( 'NONE', #17401, .T. ) ;
#5637 = FACE_OUTER_BOUND ( 'NONE', #1701, .T. ) ;
#5638 = ORIENTED_EDGE ( 'NONE', *, *, #215, .F. ) ;
#5639 = EDGE_CURVE ( 'NONE', #22814, #21354, #4804, .T. ) ;
#5640 = EDGE_LOOP ( 'NONE', ( #21371, #19934, #22682, #17696 ) ) ;
#5641 = LINE ( 'NONE', #12890, #2379 ) ;
#5642 = DIRECTION ( 'NONE',  ( -2.982858504577319616E-17, 2.441916418604790135E-15, 1.000000000000000000 ) ) ;
#5643 = VERTEX_POINT ( 'NONE', #23073 ) ;
#5644 = CARTESIAN_POINT ( 'NONE',  ( 43.84419854219520829, -33.09999999999998721, -65.86501949894326913 ) ) ;
#5645 = EDGE_CURVE ( 'NONE', #9333, #18146, #6959, .T. ) ;
#5646 = ORIENTED_EDGE ( 'NONE', *, *, #16627, .F. ) ;
#5647 = CARTESIAN_POINT ( 'NONE',  ( -27.00000000000000000, -20.00000000000000000, 2.500000000000000000 ) ) ;
#5648 = COORDINATED_UNIVERSAL_TIME_OFFSET ( 0, 0, .AHEAD. ) ;
#5649 = CARTESIAN_POINT ( 'NONE',  ( 35.11747397072455357, 7.763535785894623231, -8.759424124906624698 ) ) ;
#5650 = ADVANCED_FACE ( 'NONE', ( #17518 ), #1108, .T. ) ;
#5651 = PERSON_AND_ORGANIZATION ( #20674, #22033 ) ;
#5652 = ORIENTED_EDGE ( 'NONE', *, *, #19429, .F. ) ;
#5653 = LOCAL_TIME ( 14, 11, 27.00000000000000000, #6277 ) ;
#5654 = DIRECTION ( 'NONE',  ( -1.000000000000000000, 2.270069654138870255E-15, 0.000000000000000000 ) ) ;
#5655 = AXIS2_PLACEMENT_3D ( 'NONE', #11231, #21643, #2170 ) ;
#5656 = ORIENTED_EDGE ( 'NONE', *, *, #16144, .F. ) ;
#5657 = FACE_OUTER_BOUND ( 'NONE', #22187, .T. ) ;
#5658 = ORIENTED_EDGE ( 'NONE', *, *, #21355, .F. ) ;
#5659 = CARTESIAN_POINT ( 'NONE',  ( 69.48351927594264055, 14.58848926887901065, 1.155720087641903136E-14 ) ) ;
#5660 = LINE ( 'NONE', #304, #10727 ) ;
#5661 = DIRECTION ( 'NONE',  ( 0.000000000000000000, 0.000000000000000000, 1.000000000000000000 ) ) ;
#5662 = ORIENTED_EDGE ( 'NONE', *, *, #10248, .F. ) ;
#5663 = DATE_AND_TIME ( #12807, #17148 ) ;
#5664 = DIRECTION ( 'NONE',  ( -9.249283497051789705E-11, 1.000000000000000000, -2.220446048198130405E-15 ) ) ;
#5665 = ORIENTED_EDGE ( 'NONE', *, *, #15228, .T. ) ;
#5666 = CC_DESIGN_PERSON_AND_ORGANIZATION_ASSIGNMENT ( #9802, #13354, ( #11812 ) ) ;
#5667 = APPLICATION_PROTOCOL_DEFINITION ( 'international standard', 'config_control_design', 1994, #2791 ) ;
#5668 = EDGE_LOOP ( 'NONE', ( #12889, #2095, #17613, #4719 ) ) ;
#5669 = ORIENTED_EDGE ( 'NONE', *, *, #18407, .T. ) ;
#5670 = DIRECTION ( 'NONE',  ( 1.466984912809907930E-16, 2.805478249466195144E-20, 1.000000000000000000 ) ) ;
#5671 = CIRCLE ( 'NONE', #19345, 2.600000000000000089 ) ;
#5672 = APPROVAL_STATUS ( 'not_yet_approved' ) ;
#5673 = CIRCLE ( 'NONE', #18964, 15.25000000000000000 ) ;
#5674 = DIRECTION ( 'NONE',  ( 0.000000000000000000, 0.000000000000000000, 1.000000000000000000 ) ) ;
#5675 = PERSON_AND_ORGANIZATION_ROLE ( 'classification_officer' ) ;
#5676 = DIRECTION ( 'NONE',  ( -6.123237831918399306E-17, 1.569224110909209817E-30, 1.000000000000000000 ) ) ;
#5677 = AXIS2_PLACEMENT_3D ( 'NONE', #4913, #3133, #8715 ) ;
#5678 = LINE ( 'NONE', #1762, #15669 ) ;
#5679 = EDGE_CURVE ( 'NONE', #21097, #11071, #1091, .T. ) ;
#5680 = PERSON_AND_ORGANIZATION ( #11966, #8758 ) ;
#5681 = PRODUCT_DEFINITION_SHAPE ( 'NONE', 'NONE',  #23506 ) ;
#5682 = LOCAL_TIME ( 14, 11, 27.00000000000000000, #800 ) ;
#5683 = ORIENTED_EDGE ( 'NONE', *, *, #21420, .T. ) ;
#5684 =( GEOMETRIC_REPRESENTATION_CONTEXT ( 3 ) GLOBAL_UNCERTAINTY_ASSIGNED_CONTEXT ( ( #23423 ) ) GLOBAL_UNIT_ASSIGNED_CONTEXT ( ( #7374, #18413, #22181 ) ) REPRESENTATION_CONTEXT ( 'NONE', 'WORKASPACE' ) );
#5685 = ORIENTED_EDGE ( 'NONE', *, *, #12479, .T. ) ;
#5686 = CARTESIAN_POINT ( 'NONE',  ( 34.80031720862070443, 11.11915057133309936, 29.25000000000000000 ) ) ;
#5687 = DIRECTION ( 'NONE',  ( -0.2306359803922084506, -0.9730401042858020100, 5.112869192352694760E-15 ) ) ;
#5688 = DIRECTION ( 'NONE',  ( -1.159535895544890222E-14, -2.167612681253619929E-15, -1.000000000000000000 ) ) ;
#5689 = ORIENTED_EDGE ( 'NONE', *, *, #11292, .T. ) ;
#5690 = ORIENTED_EDGE ( 'NONE', *, *, #1280, .F. ) ;
#5691 = FACE_BOUND ( 'NONE', #3299, .T. ) ;
#5692 = EDGE_LOOP ( 'NONE', ( #12860, #2988, #22621 ) ) ;
#5693 = CIRCLE ( 'NONE', #5310, 8.250000000000000000 ) ;
#5694 = EDGE_CURVE ( 'NONE', #20737, #4894, #17640, .T. ) ;
#5695 = ADVANCED_FACE ( 'NONE', ( #5152 ), #12314, .F. ) ;
#5696 = APPLICATION_PROTOCOL_DEFINITION ( 'international standard', 'config_control_design', 1994, #8412 ) ;
#5697 = ORIENTED_EDGE ( 'NONE', *, *, #9792, .T. ) ;
#5698 = EDGE_LOOP ( 'NONE', ( #21989, #20663 ) ) ;
#5699 = CARTESIAN_POINT ( 'NONE',  ( 39.97055191974253319, 24.76972652399809149, -13.00000000000049916 ) ) ;
#5700 = VECTOR ( 'NONE', #15355, 1000.000000000000000 ) ;
#5701 = DIRECTION ( 'NONE',  ( 0.000000000000000000, 1.000000000000000000, 0.000000000000000000 ) ) ;
#5702 = DATE_AND_TIME ( #7502, #16384 ) ;
#5703 = CARTESIAN_POINT ( 'NONE',  ( 28.67817383939640052, -0.7594070262927701265, -11.00000000000039968 ) ) ;
#5704 = APPROVAL_PERSON_ORGANIZATION ( #12041, #17382, #16048 ) ;
#5705 = PLANE ( 'NONE',  #17078 ) ;
#5706 = APPROVAL_PERSON_ORGANIZATION ( #5891, #12579, #649 ) ;
#5707 = SHAPE_REPRESENTATION_RELATIONSHIP ( 'NONE' , 'NONE' ,  #11914, #567 ) ;
#5708 = CIRCLE ( 'NONE', #19743, 0.1000000000000028644 ) ;
#5709 = VERTEX_POINT ( 'NONE', #1344 ) ;
#5710 = CARTESIAN_POINT ( 'NONE',  ( 3.499952022866071211, 0.01832587339492647641, -8.931114213653268455E-14 ) ) ;
#5711 = EDGE_CURVE ( 'NONE', #9929, #18262, #20447, .T. ) ;
#5712 = COORDINATED_UNIVERSAL_TIME_OFFSET ( 0, 0, .AHEAD. ) ;
#5713 = ORIENTED_EDGE ( 'NONE', *, *, #18190, .F. ) ;
#5714 = CARTESIAN_POINT ( 'NONE',  ( -26.68881687192900287, -6.639832696913689603, 2.500292893218899692 ) ) ;
#5715 = CARTESIAN_POINT ( 'NONE',  ( 36.05760157943842614, 11.72988078058856942, -10.50000000000050981 ) ) ;
#5716 = CLOSED_SHELL ( 'NONE', ( #656, #22688, #2679, #14449, #21742, #10124, #11676, #7392, #12455, #19, #4582, #15729, #14673, #20056, #12454, #17543, #15742, #13285 ) ) ;
#5717 = CC_DESIGN_PERSON_AND_ORGANIZATION_ASSIGNMENT ( #4256, #4491, ( #1928 ) ) ;
#5718 = DIRECTION ( 'NONE',  ( 0.1153179901961009640, 0.4865200521429018377, 0.8660254037844385966 ) ) ;
#5719 = CC_DESIGN_APPROVAL ( #10557, ( #8400 ) ) ;
#5720 = CARTESIAN_POINT ( 'NONE',  ( 37.27955344062029752, 9.375336445360789028, 28.46999999999999886 ) ) ;
#5721 = CC_DESIGN_PERSON_AND_ORGANIZATION_ASSIGNMENT ( #12503, #23293, ( #795 ) ) ;
#5722 = LINE ( 'NONE', #7753, #22457 ) ;
#5723 = APPROVAL_PERSON_ORGANIZATION ( #1913, #2625, #1687 ) ;
#5724 = ORIENTED_EDGE ( 'NONE', *, *, #10517, .T. ) ;
#5725 = DIRECTION ( 'NONE',  ( -1.000000000000000000, 0.000000000000000000, 0.000000000000000000 ) ) ;
#5726 = EDGE_CURVE ( 'NONE', #1846, #10921, #13248, .T. ) ;
#5727 = EDGE_CURVE ( 'NONE', #3945, #8426, #1579, .T. ) ;
#5728 = CIRCLE ( 'NONE', #21277, 3.499999999999998668 ) ;
#5729 = ORIENTED_EDGE ( 'NONE', *, *, #17143, .F. ) ;
#5730 = VERTEX_POINT ( 'NONE', #8375 ) ;
#5731 = CARTESIAN_POINT ( 'NONE',  ( 28.41185834866789861, -1.882976958576060067, 13.00000000000019895 ) ) ;
#5732 = FACE_OUTER_BOUND ( 'NONE', #18895, .T. ) ;
#5733 = CC_DESIGN_SECURITY_CLASSIFICATION ( #1558, ( #23494 ) ) ;
#5734 = ORIENTED_EDGE ( 'NONE', *, *, #21739, .T. ) ;
#5735 = VECTOR ( 'NONE', #13587, 1000.000000000000114 ) ;
#5736 = DIRECTION ( 'NONE',  ( -0.9997648975362233292, -0.02168293463498010415, 0.000000000000000000 ) ) ;
#5737 = VERTEX_POINT ( 'NONE', #19412 ) ;
#5738 = FACE_BOUND ( 'NONE', #2959, .T. ) ;
#5739 = CALENDAR_DATE ( 2026, 31, 10 ) ;
#5740 = CARTESIAN_POINT ( 'NONE',  ( -20.00019857044559757, 22.95165872133759777, -5.000000000000060396 ) ) ;
#5741 = APPROVAL_PERSON_ORGANIZATION ( #19561, #7357, #19674 ) ;
#5742 = CC_DESIGN_APPROVAL ( #18236, ( #20866 ) ) ;
#5743 = AXIS2_PLACEMENT_3D ( 'NONE', #4388, #11656, #18885 ) ;
#5744 = CARTESIAN_POINT ( 'NONE',  ( 113.4570673249340018, -28.10438863268850085, -3.399999999999949729 ) ) ;
#5745 = VECTOR ( 'NONE', #8823, 1000.000000000000114 ) ;
#5746 = CARTESIAN_POINT ( 'NONE',  ( 113.2033677465029911, -29.17473274740279976, 13.00000000000000000 ) ) ;
#5747 = EDGE_CURVE ( 'NONE', #18882, #4216, #14188, .T. ) ;
#5748 = PERSON_AND_ORGANIZATION ( #11966, #8758 ) ;
#5749 = APPROVAL_PERSON_ORGANIZATION ( #2328, #5436, #414 ) ;
#5750 = FACE_BOUND ( 'NONE', #19351, .T. ) ;
#5751 = DIRECTION ( 'NONE',  ( -0.9744196363770861735, -1.527762929736005432E-17, -0.2247362281492400471 ) ) ;
#5752 = CC_DESIGN_PERSON_AND_ORGANIZATION_ASSIGNMENT ( #2229, #11646, ( #18416 ) ) ;
#5753 = CARTESIAN_POINT ( 'NONE',  ( -20.00000001831885044, -17.24999999999999645, 8.500000000004543921 ) ) ;
#5754 = CARTESIAN_POINT ( 'NONE',  ( -62.91249983789198552, 7.670697574599159907, -8.978560695896640676E-17 ) ) ;
#5755 = PRODUCT_RELATED_PRODUCT_CATEGORY ( 'detail', '', ( #21422 ) ) ;
#5756 = CARTESIAN_POINT ( 'NONE',  ( 5.000000000000000000, -30.47499999999999787, 19.00000000000000000 ) ) ;
#5757 = CARTESIAN_POINT ( 'NONE',  ( -62.93786153767959490, 12.51438117767279934, 3.385904617822409831E-15 ) ) ;
#5758 = EDGE_CURVE ( 'NONE', #8468, #4216, #15134, .T. ) ;
#5760 = ORIENTED_EDGE ( 'NONE', *, *, #20798, .T. ) ;
#5759 = EDGE_CURVE ( 'NONE', #6113, #4832, #21204, .T. ) ;
#5761 = SECURITY_CLASSIFICATION ( '', '', #19508 ) ;
#5762 = ORIENTED_EDGE ( 'NONE', *, *, #7026, .F. ) ;
#5763 = CARTESIAN_POINT ( 'NONE',  ( 35.59419854219520118, 9.774809681453278998, 25.00000000000000000 ) ) ;
#5764 = ORIENTED_EDGE ( 'NONE', *, *, #17683, .F. ) ;
#5765 = AXIS2_PLACEMENT_3D ( 'NONE', #22597, #6950, #17748 ) ;
#5766 = FACE_BOUND ( 'NONE', #20069, .T. ) ;
#5767 = ORIENTED_EDGE ( 'NONE', *, *, #8368, .F. ) ;
#5768 = VECTOR ( 'NONE', #312, 1000.000000000000000 ) ;
#5769 = AXIS2_PLACEMENT_3D ( 'NONE', #14319, #18014, #19906 ) ;
#5770 = DIRECTION ( 'NONE',  ( 0.2306359803922078122, 0.9730401042858023430, 2.478176394252582127E-15 ) ) ;
#5771 =( BOUNDED_CURVE ( )  B_SPLINE_CURVE ( 2, ( #8821, #11208, #1551 ),
 .UNSPECIFIED., .F., .F. ) 
 B_SPLINE_CURVE_WITH_KNOTS ( ( 3, 3 ),
 ( 0.1168436138077930952, 0.2336872276155859962 ),
 .UNSPECIFIED. ) 
 CURVE ( )  GEOMETRIC_REPRESENTATION_ITEM ( )  RATIONAL_B_SPLINE_CURVE ( ( 1.077350269189629950, 1.077350269189629728, 1.000000000000000000 ) ) 
 REPRESENTATION_ITEM ( '' )  );
#5772 = LINE ( 'NONE', #10603, #14129 ) ;
#5773 = PERSON_AND_ORGANIZATION ( #11966, #8758 ) ;
#5774 = CARTESIAN_POINT ( 'NONE',  ( -24.50000000000000000, -28.60000000000000142, -19.00000000000000000 ) ) ;
#5775 = AXIS2_PLACEMENT_3D ( 'NONE', #7755, #16639, #20453 ) ;
#5776 = APPROVAL_STATUS ( 'not_yet_approved' ) ;
#5777 = AXIS2_PLACEMENT_3D ( 'NONE', #11432, #13312, #22087 ) ;
#5778 = SHAPE_REPRESENTATION_RELATIONSHIP ( 'NONE' , 'NONE' ,  #2026, #21806 ) ;
#5779 = CARTESIAN_POINT ( 'NONE',  ( -0.7498608572560920837, 18.38930330212339825, -2.632567431446439807E-17 ) ) ;
#5780 = ORIENTED_EDGE ( 'NONE', *, *, #23303, .F. ) ;
#5781 = EDGE_CURVE ( 'NONE', #1005, #2908, #12143, .T. ) ;
#5782 = LOCAL_TIME ( 14, 11, 27.00000000000000000, #1273 ) ;
#5783 = FACE_OUTER_BOUND ( 'NONE', #17641, .T. ) ;
#5784 = AXIS2_PLACEMENT_3D ( 'NONE', #14150, #3680, #1892 ) ;
#5785 = ORIENTED_EDGE ( 'NONE', *, *, #5330, .F. ) ;
#5786 = CARTESIAN_POINT ( 'NONE',  ( 118.6002496876800052, -6.405594307115080710, -18.89999999999999858 ) ) ;
#5787 = VECTOR ( 'NONE', #991, 1000.000000000000114 ) ;
#5788 = AXIS2_PLACEMENT_3D ( 'NONE', #288, #1845, #16332 ) ;
#5789 = CARTESIAN_POINT ( 'NONE',  ( 39.67523673029199927, 5.313293424922060026, -18.89999999999999858 ) ) ;
#5790 = ORIENTED_EDGE ( 'NONE', *, *, #20292, .T. ) ;
#5791 = DIRECTION ( 'NONE',  ( -1.000000000000000000, 0.000000000000000000, 0.000000000000000000 ) ) ;
#5792 = DIRECTION ( 'NONE',  ( 0.1630842657209385649, 0.6880432561069587116, 0.7071067811865449082 ) ) ;
#5793 = CARTESIAN_POINT ( 'NONE',  ( 27.03882233449100170, -4.640652085158319728, 20.00000000000000000 ) ) ;
#5794 = ORIENTED_EDGE ( 'NONE', *, *, #21285, .F. ) ;
#5795 = APPLICATION_CONTEXT ( 'configuration controlled 3d designs of mechanical parts and assemblies' ) ;
#5796 = ADVANCED_FACE ( 'NONE', ( #7072 ), #12187, .F. ) ;
#5797 = VECTOR ( 'NONE', #397, 1000.000000000000000 ) ;
#5798 = DATE_TIME_ROLE ( 'classification_date' ) ;
#5799 = ADVANCED_FACE ( 'NONE', ( #11963 ), #22962, .T. ) ;
#5800 = CARTESIAN_POINT ( 'NONE',  ( 35.11747397072451804, 7.763535785894483787, -37.44562646538079065 ) ) ;
#5801 = AXIS2_PLACEMENT_3D ( 'NONE', #7240, #5215, #7020 ) ;
#5802 = EDGE_LOOP ( 'NONE', ( #16480, #3067, #3789, #21821 ) ) ;
#5803 = AXIS2_PLACEMENT_3D ( 'NONE', #9495, #19949, #14953 ) ;
#5804 = APPROVAL_STATUS ( 'not_yet_approved' ) ;
#5805 = LINE ( 'NONE', #3343, #15640 ) ;
#5806 = LOCAL_TIME ( 14, 11, 27.00000000000000000, #4107 ) ;
#5807 = EDGE_LOOP ( 'NONE', ( #16764, #9220, #11543, #16078 ) ) ;
#5808 = VERTEX_POINT ( 'NONE', #4922 ) ;
#5809 = CARTESIAN_POINT ( 'NONE',  ( 37.10730959030829723, 23.96304573415820016, 15.00000000000000000 ) ) ;
#5810 = COORDINATED_UNIVERSAL_TIME_OFFSET ( 0, 0, .AHEAD. ) ;
#5811 = AXIS2_PLACEMENT_3D ( 'NONE', #23254, #18039, #6884 ) ;
#5812 = AXIS2_PLACEMENT_3D ( 'NONE', #13567, #5860, #11230 ) ;
#5813 = AXIS2_PLACEMENT_3D ( 'NONE', #22476, #6224, #19047 ) ;
#5814 = DIRECTION ( 'NONE',  ( 1.000000000000000000, -2.099364410518905248E-23, -2.269747374240930013E-13 ) ) ;
#5815 = APPROVAL_ROLE ( '' ) ;
#5816 = CARTESIAN_POINT ( 'NONE',  ( 28.07896398525729964, -3.287439373930340025, 11.50000000000019895 ) ) ;
#5818 = AXIS2_PLACEMENT_3D ( 'NONE', #5115, #23377, #14247 ) ;
#5817 = LINE ( 'NONE', #11055, #10760 ) ;
#5819 = CC_DESIGN_PERSON_AND_ORGANIZATION_ASSIGNMENT ( #1765, #17947, ( #1510 ) ) ;
#5820 = PERSON_AND_ORGANIZATION ( #11966, #8758 ) ;
#5821 = SECURITY_CLASSIFICATION ( '', '', #513 ) ;
#5822 = ORIENTED_EDGE ( 'NONE', *, *, #1139, .T. ) ;
#5823 = AXIS2_PLACEMENT_3D ( 'NONE', #16443, #21902, #7091 ) ;
#5824 = LINE ( 'NONE', #7720, #12598 ) ;
#5825 = VERTEX_POINT ( 'NONE', #3144 ) ;
#5826 = FACE_OUTER_BOUND ( 'NONE', #5214, .T. ) ;
#5827 = CARTESIAN_POINT ( 'NONE',  ( -3.458317987535629801, 19.03127855354509990, -7.892745253163399067E-16 ) ) ;
#5828 = DIRECTION ( 'NONE',  ( 1.138590270679734009E-14, 2.220446049251240387E-15, 1.000000000000000000 ) ) ;
#5829 = VERTEX_POINT ( 'NONE', #8610 ) ;
#5830 = VERTEX_POINT ( 'NONE', #7635 ) ;
#5831 = DIRECTION ( 'NONE',  ( 0.0007613694435018767380, -0.9999997101582432935, 0.000000000000000000 ) ) ;
#5832 = EDGE_LOOP ( 'NONE', ( #11228, #8524 ) ) ;
#5833 = DATE_TIME_ROLE ( 'creation_date' ) ;
#5834 = ORIENTED_EDGE ( 'NONE', *, *, #21176, .T. ) ;
#5835 = EDGE_LOOP ( 'NONE', ( #10907, #15078, #4776, #18429 ) ) ;
#5836 = CARTESIAN_POINT ( 'NONE',  ( -59.94074421850589829, 13.07278162995702431, -5.883059113410419196E-15 ) ) ;
#5837 = VECTOR ( 'NONE', #8936, 1000.000000000000000 ) ;
#5838 = CARTESIAN_POINT ( 'NONE',  ( 118.5079952955235996, -6.794810348829486202, 3.447633465585020886E-14 ) ) ;
#5839 = APPROVAL_DATE_TIME ( #7610, #15886 ) ;
#5840 = DIRECTION ( 'NONE',  ( 3.330999558957018649E-36, 2.805478249471640109E-20, 1.000000000000000000 ) ) ;
#5841 = EDGE_CURVE ( 'NONE', #10807, #935, #7202, .T. ) ;
#5842 = AXIS2_PLACEMENT_3D ( 'NONE', #18385, #11028, #12796 ) ;
#5843 = DIRECTION ( 'NONE',  ( -1.187319687680494078E-16, -2.805478249478265308E-20, -1.000000000000000000 ) ) ;
#5844 = VECTOR ( 'NONE', #7260, 999.9999999999998863 ) ;
#5845 = ORIENTED_EDGE ( 'NONE', *, *, #11742, .F. ) ;
#5846 = FACE_OUTER_BOUND ( 'NONE', #16348, .T. ) ;
#5847 = APPLICATION_PROTOCOL_DEFINITION ( 'international standard', 'config_control_design', 1994, #9124 ) ;
#5848 = EDGE_LOOP ( 'NONE', ( #1994, #22174 ) ) ;
#5849 = DIRECTION ( 'NONE',  ( 0.000000000000000000, 0.000000000000000000, -1.000000000000000000 ) ) ;
#5850 = CARTESIAN_POINT ( 'NONE',  ( 30.50389457288209982, -2.378844316418729843, 13.00000000000000000 ) ) ;
#5851 = AXIS2_PLACEMENT_3D ( 'NONE', #2068, #42, #16210 ) ;
#5852 = DIRECTION ( 'NONE',  ( -0.9730401042858035643, 0.2306359803922028717, 5.667427308550587516E-17 ) ) ;
#5853 = DIRECTION ( 'NONE',  ( -0.005235963827101446956, 0.9999862922474495042, 5.492442074325198113E-16 ) ) ;
#5854 = ORIENTED_EDGE ( 'NONE', *, *, #13690, .T. ) ;
#5855 = VECTOR ( 'NONE', #14118, 1000.000000000000000 ) ;
#5856 = FACE_OUTER_BOUND ( 'NONE', #5121, .T. ) ;
#5857 = UNCERTAINTY_MEASURE_WITH_UNIT (LENGTH_MEASURE( 1.000000000000000082E-05 ), #8867, 'distance_accuracy_value', 'NONE');
#5858 = ORIENTED_EDGE ( 'NONE', *, *, #7249, .F. ) ;
#5859 = ORIENTED_EDGE ( 'NONE', *, *, #16091, .F. ) ;
#5860 = DIRECTION ( 'NONE',  ( 3.099353312215989243E-62, -2.689336210007789456E-77, -1.000000000000000000 ) ) ;
#5861 = CARTESIAN_POINT ( 'NONE',  ( -14.98746859791960162, 26.70208920133150343, 5.500000000004400036 ) ) ;
#5862 = ORIENTED_EDGE ( 'NONE', *, *, #3676, .T. ) ;
#5863 = PERSON_AND_ORGANIZATION ( #11966, #8758 ) ;
#5864 = CARTESIAN_POINT ( 'NONE',  ( 118.6002496876800052, -6.405594307115070052, -15.90000000000000036 ) ) ;
#5865 = ADVANCED_FACE ( 'NONE', ( #7529, #5732 ), #14537, .T. ) ;
#5866 = DIRECTION ( 'NONE',  ( -3.099353312215989243E-62, -1.872670541876879671E-92, 1.000000000000000000 ) ) ;
#5867 = CALENDAR_DATE ( 2026, 31, 10 ) ;
#5868 = CARTESIAN_POINT ( 'NONE',  ( -19.99999999999849720, -20.00000000000000000, -8.749999999995610622 ) ) ;
#5869 = CC_DESIGN_DATE_AND_TIME_ASSIGNMENT ( #6127, #20624, ( #13727 ) ) ;
#5870 =( NAMED_UNIT ( * ) PLANE_ANGLE_UNIT ( ) SI_UNIT ( $, .RADIAN. ) );
#5871 = LINE ( 'NONE', #20352, #8099 ) ;
#5872 = EDGE_CURVE ( 'NONE', #11260, #10096, #16650, .T. ) ;
#5873 = EDGE_CURVE ( 'NONE', #17258, #1544, #18211, .T. ) ;
#5874 = DIRECTION ( 'NONE',  ( -2.269700743865584947E-13, -2.220446049247695246E-15, -1.000000000000000000 ) ) ;
#5875 = COORDINATED_UNIVERSAL_TIME_OFFSET ( 0, 0, .AHEAD. ) ;
#5876 = CARTESIAN_POINT ( 'NONE',  ( -32.42710143188249816, 10.33427914179039853, 3.750000000000000000 ) ) ;
#5877 = DIRECTION ( 'NONE',  ( -1.751019220569994795E-16, -2.300154215587015208E-15, -1.000000000000000000 ) ) ;
#5878 = DIRECTION ( 'NONE',  ( -0.9730401042858035643, 0.2306359803922028717, 5.958148513035547083E-17 ) ) ;
#5879 = FACE_OUTER_BOUND ( 'NONE', #19039, .T. ) ;
#5880 = CARTESIAN_POINT ( 'NONE',  ( 31.45181451370270054, 16.90945435098589655, -25.00000000000000000 ) ) ;
#5881 = ORIENTED_EDGE ( 'NONE', *, *, #15746, .F. ) ;
#5882 = AXIS2_PLACEMENT_3D ( 'NONE', #10825, #1878, #1758 ) ;
#5883 = VERTEX_POINT ( 'NONE', #5507 ) ;
#5884 = CARTESIAN_POINT ( 'NONE',  ( -62.94391562085439773, 13.67061532808409829, -5.515300856952130332E-15 ) ) ;
#5885 = FACE_OUTER_BOUND ( 'NONE', #12387, .T. ) ;
#5886 = ORIENTED_EDGE ( 'NONE', *, *, #3911, .F. ) ;
#5887 = FACE_OUTER_BOUND ( 'NONE', #21368, .T. ) ;
#5888 = EDGE_CURVE ( 'NONE', #4401, #14881, #12526, .T. ) ;
#5889 = ORIENTED_EDGE ( 'NONE', *, *, #19486, .T. ) ;
#5890 = CARTESIAN_POINT ( 'NONE',  ( -26.99999999999959854, -19.33065833018799751, -25.00000000000000000 ) ) ;
#5891 = PERSON_AND_ORGANIZATION ( #11966, #8758 ) ;
#5892 = CARTESIAN_POINT ( 'NONE',  ( 37.65622438626208890, 9.971723439402808253, -8.976109897029356688 ) ) ;
#5893 = PRODUCT_DEFINITION ( 'UNKNOWN', '', #14124, #10898 ) ;
#5894 = PRODUCT_DEFINITION_SHAPE ( 'NONE', 'NONE',  #23503 ) ;
#5895 = CC_DESIGN_PERSON_AND_ORGANIZATION_ASSIGNMENT ( #13628, #1267, ( #21034 ) ) ;
#5896 = ITEM_DEFINED_TRANSFORMATION ( 'NONE', 'NONE', #2887,  #12739 ) ;
#5897 = DIRECTION ( 'NONE',  ( -0.2306359803922085339, -0.9730401042858022320, 0.000000000000000000 ) ) ;
#5898 = ADVANCED_FACE ( 'NONE', ( #14648 ), #16643, .T. ) ;
#5899 = EDGE_CURVE ( 'NONE', #2851, #13535, #19333, .T. ) ;
#5900 = EDGE_LOOP ( 'NONE', ( #13710, #1197, #20809, #10641 ) ) ;
#5901 = CC_DESIGN_DATE_AND_TIME_ASSIGNMENT ( #2279, #20804, ( #1527 ) ) ;
#5902 = CYLINDRICAL_SURFACE ( 'NONE', #22513, 2.499999999999999112 ) ;
#5903 = ORIENTED_EDGE ( 'NONE', *, *, #15808, .T. ) ;
#5904 = DIRECTION ( 'NONE',  ( -0.7070970883417647679, -0.003702385528188428636, -0.7071067811865467956 ) ) ;
#5905 = DIRECTION ( 'NONE',  ( 2.269747459789000104E-13, 2.220446049250330436E-15, 1.000000000000000000 ) ) ;
#5906 = ORIENTED_EDGE ( 'NONE', *, *, #5600, .T. ) ;
#5907 = LINE ( 'NONE', #20393, #8994 ) ;
#5908 = CARTESIAN_POINT ( 'NONE',  ( 3.499952022866072543, 0.01832587339492648335, -2.500000000000090594 ) ) ;
#5909 = CARTESIAN_POINT ( 'NONE',  ( 36.12085580342079538, 11.99674675959015246, 19.78349999999998943 ) ) ;
#5910 = EDGE_LOOP ( 'NONE', ( #3309, #20582 ) ) ;
#5911 = CARTESIAN_POINT ( 'NONE',  ( 105.8171986446039909, -20.23006919877430221, -13.00000000000000000 ) ) ;
#5912 = ORIENTED_EDGE ( 'NONE', *, *, #14280, .T. ) ;
#5913 = DATE_AND_TIME ( #4248, #7282 ) ;
#5914 = CARTESIAN_POINT ( 'NONE',  ( -27.00000000000000000, -28.60000000000000142, 21.50000000000000000 ) ) ;
#5915 = EDGE_CURVE ( 'NONE', #12721, #5825, #19992, .T. ) ;
#5916 = ORIENTED_EDGE ( 'NONE', *, *, #14511, .T. ) ;
#5917 = ORIENTED_EDGE ( 'NONE', *, *, #18591, .T. ) ;
#5918 = DIRECTION ( 'NONE',  ( -0.9999862922474492821, -0.005235963827121953122, 1.239088197126291310E-16 ) ) ;
#5919 = COORDINATED_UNIVERSAL_TIME_OFFSET ( 0, 0, .AHEAD. ) ;
#5920 = VECTOR ( 'NONE', #6899, 1000.000000000000114 ) ;
#5921 = PERSON_AND_ORGANIZATION_ROLE ( 'classification_officer' ) ;
#5922 = DIRECTION ( 'NONE',  ( -2.269747459788994803E-13, -2.220446049250330436E-15, -1.000000000000000000 ) ) ;
#5923 = EDGE_CURVE ( 'NONE', #20782, #12824, #10989, .T. ) ;
#5924 = EDGE_CURVE ( 'NONE', #1782, #22209, #18179, .T. ) ;
#5925 = CARTESIAN_POINT ( 'NONE',  ( 111.8137341348020044, 5.068973512656540059, -13.00000000000000000 ) ) ;
#5926 = COORDINATED_UNIVERSAL_TIME_OFFSET ( 0, 0, .AHEAD. ) ;
#5927 = VECTOR ( 'NONE', #16281, 1000.000000000000000 ) ;
#5928 = CIRCLE ( 'NONE', #13901, 2.749999999999999112 ) ;
#5929 = ORIENTED_EDGE ( 'NONE', *, *, #1133, .F. ) ;
#5930 = DIRECTION ( 'NONE',  ( -0.7273594590164595974, 0.6862566701892837129, -3.292724291071135063E-15 ) ) ;
#5931 = ORIENTED_EDGE ( 'NONE', *, *, #10263, .F. ) ;
#5932 = DIRECTION ( 'NONE',  ( 2.982858504489129897E-17, -2.441916418604790135E-15, -1.000000000000000000 ) ) ;
#5933 = PLANE ( 'NONE',  #17222 ) ;
#5934 = DIRECTION ( 'NONE',  ( -1.000000000000000000, -6.662111140531837817E-09, 1.144917494144693313E-14 ) ) ;
#5935 = ORIENTED_EDGE ( 'NONE', *, *, #23032, .T. ) ;
#5936 = ORIENTED_EDGE ( 'NONE', *, *, #4970, .T. ) ;
#5937 = CARTESIAN_POINT ( 'NONE',  ( -0.03653820904331969710, 20.46006235366549575, -4.500000000000000000 ) ) ;
#5938 = VERTEX_POINT ( 'NONE', #21526 ) ;
#5939 = PERSON_AND_ORGANIZATION_ROLE ( 'creator' ) ;
#5940 = EDGE_LOOP ( 'NONE', ( #10717, #20748, #12358, #11533 ) ) ;
#5941 = VERTEX_POINT ( 'NONE', #9189 ) ;
#5942 = CARTESIAN_POINT ( 'NONE',  ( -24.50000000000000000, -31.09999999999999787, 19.00000000000000000 ) ) ;
#5943 = LINE ( 'NONE', #19213, #13570 ) ;
#5944 = DATE_AND_TIME ( #7735, #12231 ) ;
#5945 = CARTESIAN_POINT ( 'NONE',  ( -29.02403449025189985, 6.348118223725100151, -4.767474059747799586 ) ) ;
#5946 = CIRCLE ( 'NONE', #6339, 5.000000000000000888 ) ;
#5947 = CARTESIAN_POINT ( 'NONE',  ( -30.79248430819439974, 6.338858557519069237, -2.999000000000079602 ) ) ;
#5948 = VECTOR ( 'NONE', #16007, 1000.000000000000000 ) ;
#5949 = CIRCLE ( 'NONE', #630, 0.5000000000000004441 ) ;
#5950 = EDGE_CURVE ( 'NONE', #22077, #1934, #7296, .T. ) ;
#5951 = EDGE_CURVE ( 'NONE', #15133, #19473, #21954, .T. ) ;
#5952 = ORIENTED_EDGE ( 'NONE', *, *, #12764, .F. ) ;
#5953 = CARTESIAN_POINT ( 'NONE',  ( 122.4288069621910040, 9.746871424029221131, -10.02499999999999858 ) ) ;
#5954 = DATE_AND_TIME ( #7858, #19769 ) ;
#5955 = ORIENTED_EDGE ( 'NONE', *, *, #15228, .F. ) ;
#5956 = AXIS2_PLACEMENT_3D ( 'NONE', #12749, #3479, #10754 ) ;
#5957 = CYLINDRICAL_SURFACE ( 'NONE', #6854, 2.750000000000000888 ) ;
#5958 = DIRECTION ( 'NONE',  ( -2.269700743865584947E-13, -2.220446049247695246E-15, -1.000000000000000000 ) ) ;
#5959 = VERTEX_POINT ( 'NONE', #18342 ) ;
#5960 = AXIS2_PLACEMENT_3D ( 'NONE', #5272, #12534, #9314 ) ;
#5961 = DIRECTION ( 'NONE',  ( -0.2306359803922026497, -0.9730401042858035643, 0.000000000000000000 ) ) ;
#5962 = AXIS2_PLACEMENT_3D ( 'NONE', #19151, #10024, #17252 ) ;
#5963 = FACE_OUTER_BOUND ( 'NONE', #7384, .T. ) ;
#5964 = EDGE_LOOP ( 'NONE', ( #22787, #22650, #18178, #5952, #12618, #15544 ) ) ;
#5965 = PLANE ( 'NONE',  #15646 ) ;
#5966 = PERSON_AND_ORGANIZATION ( #11966, #8758 ) ;
#5967 = ORIENTED_EDGE ( 'NONE', *, *, #14610, .T. ) ;
#5968 = VERTEX_POINT ( 'NONE', #20233 ) ;
#5969 = DIRECTION ( 'NONE',  ( -0.9730401042858036753, 0.2306359803922028995, 5.958148513035547083E-17 ) ) ;
#5970 = PLANE ( 'NONE',  #16723 ) ;
#5971 = CIRCLE ( 'NONE', #9015, 2.066999999999999726 ) ;
#5972 = APPLICATION_CONTEXT ( 'configuration controlled 3d designs of mechanical parts and assemblies' ) ;
#5973 = VERTEX_POINT ( 'NONE', #12864 ) ;
#5974 = MECHANICAL_CONTEXT ( 'NONE', #608, 'mechanical' ) ;
#5975 = LINE ( 'NONE', #20463, #11911 ) ;
#5976 = CARTESIAN_POINT ( 'NONE',  ( -14.54830929633950021, -2.787889851644880235, -5.499999999996740385 ) ) ;
#5977 = CIRCLE ( 'NONE', #10172, 2.500000000000000000 ) ;
#5978 = DATE_AND_TIME ( #9684, #875 ) ;
#5979 = FACE_OUTER_BOUND ( 'NONE', #14686, .T. ) ;
#5980 = VECTOR ( 'NONE', #9832, 1000.000000000000000 ) ;
#5981 = AXIS2_PLACEMENT_3D ( 'NONE', #13693, #6095, #8006 ) ;
#5982 = VECTOR ( 'NONE', #11356, 1000.000000000000227 ) ;
#5983 = SHAPE_REPRESENTATION_RELATIONSHIP ( 'NONE' , 'NONE' ,  #9605, #5414 ) ;
#5984 = DIRECTION ( 'NONE',  ( -1.000000000000000000, 0.000000000000000000, 0.000000000000000000 ) ) ;
#5985 = CARTESIAN_POINT ( 'NONE',  ( -20.00000000397360012, 22.95208919256889857, -5.000000000000000000 ) ) ;
#5986 = DATE_TIME_ROLE ( 'creation_date' ) ;
#5987 = LINE ( 'NONE', #8013, #2436 ) ;
#5988 = CIRCLE ( 'NONE', #16232, 5.000000000000000888 ) ;
#5989 = CARTESIAN_POINT ( 'NONE',  ( 35.59419854219520118, 9.774809681453358934, -10.50000000000050093 ) ) ;
#5990 = EDGE_CURVE ( 'NONE', #20926, #12435, #714, .T. ) ;
#5991 = LINE ( 'NONE', #9696, #1380 ) ;
#5992 = ADVANCED_FACE ( 'NONE', ( #3830, #3960 ), #21774, .F. ) ;
#5993 = FACE_BOUND ( 'NONE', #23430, .T. ) ;
#5994 = AXIS2_PLACEMENT_3D ( 'NONE', #10220, #13645, #22658 ) ;
#5995 = CYLINDRICAL_SURFACE ( 'NONE', #6597, 2.500000000000000444 ) ;
#5996 = DIRECTION ( 'NONE',  ( -6.662111519016958720E-09, 1.000000000000000000, -2.523234146875356491E-15 ) ) ;
#5997 = ORIENTED_EDGE ( 'NONE', *, *, #350, .T. ) ;
#5998 = EDGE_LOOP ( 'NONE', ( #11906, #20666 ) ) ;
#5999 = DIRECTION ( 'NONE',  ( -0.9999862922474493931, -0.005235963827107929618, 0.000000000000000000 ) ) ;
#6000 = AXIS2_PLACEMENT_3D ( 'NONE', #19054, #13698, #15719 ) ;
#6001 = CARTESIAN_POINT ( 'NONE',  ( 113.4570673249340018, -28.10438863268850085, -2.700000000000000178 ) ) ;
#6002 = ORIENTED_EDGE ( 'NONE', *, *, #5951, .F. ) ;
#6003 = EDGE_CURVE ( 'NONE', #2081, #19473, #16194, .T. ) ;
#6004 = ADVANCED_FACE ( 'NONE', ( #14407 ), #19887, .F. ) ;
#6005 = CARTESIAN_POINT ( 'NONE',  ( -20.00000000397360012, 22.95208919256889857, -2.500000000000039968 ) ) ;
#6006 = EDGE_LOOP ( 'NONE', ( #10670, #3178, #2837, #10695, #4977, #21848, #5611, #11586, #1446 ) ) ;
#6007 = DIRECTION ( 'NONE',  ( 0.9730401042858023430, -0.2306359803922080620, -5.959266323858946149E-17 ) ) ;
#6008 = CALENDAR_DATE ( 2026, 31, 10 ) ;
#6009 = CARTESIAN_POINT ( 'NONE',  ( 35.87511680767506306, 27.43616820587386229, 13.00000000000000000 ) ) ;
#6010 = CALENDAR_DATE ( 2026, 31, 10 ) ;
#6011 = CARTESIAN_POINT ( 'NONE',  ( -19.19277407259999180, 26.35772955756921121, -2.500000000000000000 ) ) ;
#6012 = ORIENTED_EDGE ( 'NONE', *, *, #4421, .F. ) ;
#6013 = AXIS2_PLACEMENT_3D ( 'NONE', #7804, #548, #421 ) ;
#6014 = DIRECTION ( 'NONE',  ( 3.099353312215989243E-62, 1.872670541876879671E-92, -1.000000000000000000 ) ) ;
#6015 = ORIENTED_EDGE ( 'NONE', *, *, #4147, .F. ) ;
#6016 = DIRECTION ( 'NONE',  ( -0.005235963827102643048, 0.9999862922474495042, 7.724582913192744961E-15 ) ) ;
#6017 = EDGE_CURVE ( 'NONE', #2028, #18242, #22119, .T. ) ;
#6018 = DIRECTION ( 'NONE',  ( -0.2306359803922028440, -0.9730401042858034533, -4.307366329831518561E-32 ) ) ;
#6019 = ORIENTED_EDGE ( 'NONE', *, *, #3696, .F. ) ;
#6020 = LINE ( 'NONE', #13619, #3300 ) ;
#6021 = DIRECTION ( 'NONE',  ( 0.2306359803922022056, 0.9730401042858037863, -4.163336342344340971E-15 ) ) ;
#6022 = VERTEX_POINT ( 'NONE', #4536 ) ;
#6023 = CC_DESIGN_PERSON_AND_ORGANIZATION_ASSIGNMENT ( #3494, #21432, ( #22114 ) ) ;
#6024 = APPROVAL_DATE_TIME ( #22046, #22683 ) ;
#6025 = APPROVAL ( #19863, 'UNSPECIFIED' ) ;
#6026 = CARTESIAN_POINT ( 'NONE',  ( -68.51547434528259828, -24.91260405369630249, -2.885287058652779450E-14 ) ) ;
#6027 = ORIENTED_EDGE ( 'NONE', *, *, #919, .T. ) ;
#6028 = EDGE_CURVE ( 'NONE', #10063, #23388, #12511, .T. ) ;
#6029 = EDGE_CURVE ( 'NONE', #6605, #19111, #9852, .T. ) ;
#6030 = SECURITY_CLASSIFICATION_LEVEL ( 'unclassified' ) ;
#6031 = CARTESIAN_POINT ( 'NONE',  ( -20.00000000397270128, 22.95208919257349933, 6.750000000004470202 ) ) ;
#6032 = VERTEX_POINT ( 'NONE', #8124 ) ;
#6033 = VERTEX_POINT ( 'NONE', #7875 ) ;
#6034 = CARTESIAN_POINT ( 'NONE',  ( -62.93704341833160498, 12.35813331950920002, -2.458500000000113150 ) ) ;
#6035 = PERSON_AND_ORGANIZATION ( #11966, #8758 ) ;
#6036 = PERSON_AND_ORGANIZATION ( #2241, #18946 ) ;
#6037 = DIRECTION ( 'NONE',  ( 1.000000000000000000, 9.250482324585361611E-11, -2.269018306577663175E-13 ) ) ;
#6038 = TOROIDAL_SURFACE ( 'NONE', #19741, 2.380000000000000338, 2.370000000000000107 ) ;
#6039 =( NAMED_UNIT ( * ) SI_UNIT ( $, .STERADIAN. ) SOLID_ANGLE_UNIT ( ) );
#6040 = CARTESIAN_POINT ( 'NONE',  ( 113.2033677465029911, -29.17473274740279976, 3.100000000000039613 ) ) ;
#6041 = VERTEX_POINT ( 'NONE', #13111 ) ;
#6042 = APPROVAL_DATE_TIME ( #209, #7944 ) ;
#6043 = ADVANCED_FACE ( 'NONE', ( #4324 ), #14993, .F. ) ;
#6044 = ORIENTED_EDGE ( 'NONE', *, *, #23294, .F. ) ;
#6045 = FACE_OUTER_BOUND ( 'NONE', #7125, .T. ) ;
#6046 = ORIENTED_EDGE ( 'NONE', *, *, #8571, .T. ) ;
#6047 = LINE ( 'NONE', #13300, #2593 ) ;
#6048 = CARTESIAN_POINT ( 'NONE',  ( 55.46237324781409939, -8.294657213477510282, 13.00000000000000000 ) ) ;
#6049 = CARTESIAN_POINT ( 'NONE',  ( -60.06514239919540188, -6.814592325618320068, -3.000000000000079936 ) ) ;
#6050 = VERTEX_POINT ( 'NONE', #11465 ) ;
#6051 = LOCAL_TIME ( 14, 11, 27.00000000000000000, #11817 ) ;
#6052 = VERTEX_POINT ( 'NONE', #2768 ) ;
#6054 = DIRECTION ( 'NONE',  ( -0.2306359803922033991, -0.9730401042858033422, 0.000000000000000000 ) ) ;
#6053 = AXIS2_PLACEMENT_3D ( 'NONE', #19042, #16892, #11590 ) ;
#6055 = ORIENTED_EDGE ( 'NONE', *, *, #11608, .F. ) ;
#6056 = ADVANCED_FACE ( 'NONE', ( #22580 ), #615, .F. ) ;
#6057 = EDGE_CURVE ( 'NONE', #14376, #20293, #11349, .T. ) ;
#6058 = SECURITY_CLASSIFICATION_LEVEL ( 'unclassified' ) ;
#6059 = ORIENTED_EDGE ( 'NONE', *, *, #8008, .T. ) ;
#6060 = ORIENTED_EDGE ( 'NONE', *, *, #14192, .T. ) ;
#6061 = CARTESIAN_POINT ( 'NONE',  ( 37.03119170130820237, 10.20498483259809497, -27.44000000000050576 ) ) ;
#6062 = DATE_AND_TIME ( #4293, #6153 ) ;
#6063 = CARTESIAN_POINT ( 'NONE',  ( 102.3363885986873356, 5.191082435725784983, -13.00000000000000000 ) ) ;
#6064 = DIRECTION ( 'NONE',  ( 0.2306359803922076457, 0.9730401042858025651, -1.412237191019970710E-17 ) ) ;
#6065 =( LENGTH_UNIT ( ) NAMED_UNIT ( * ) SI_UNIT ( .MILLI., .METRE. ) );
#6066 = AXIS2_PLACEMENT_3D ( 'NONE', #12081, #17039, #8265 ) ;
#6067 = CIRCLE ( 'NONE', #3406, 2.066999999999999726 ) ;
#6068 = CARTESIAN_POINT ( 'NONE',  ( -27.00000000000000000, -31.09999999999999787, 21.50000000000000000 ) ) ;
#6069 = APPLICATION_PROTOCOL_DEFINITION ( 'international standard', 'config_control_design', 1994, #6706 ) ;
#6070 = EDGE_CURVE ( 'NONE', #20686, #7111, #140, .T. ) ;
#6071 = EDGE_LOOP ( 'NONE', ( #19780, #15351, #4628, #7743 ) ) ;
#6072 = DIRECTION ( 'NONE',  ( -0.005235963827102643048, 0.9999862922474495042, -7.723249237701186312E-15 ) ) ;
#6073 = PLANE ( 'NONE',  #2147 ) ;
#6074 = AXIS2_PLACEMENT_3D ( 'NONE', #22105, #7621, #14981 ) ;
#6075 = ORIENTED_EDGE ( 'NONE', *, *, #22865, .T. ) ;
#6076 = DIRECTION ( 'NONE',  ( 0.2306359803922084506, 0.9730401042858022320, -5.112869192352694760E-15 ) ) ;
#6077 = FACE_BOUND ( 'NONE', #5311, .T. ) ;
#6078 = CIRCLE ( 'NONE', #22377, 2.500999999999639734 ) ;
#6079 = ORIENTED_EDGE ( 'NONE', *, *, #18745, .F. ) ;
#6080 = DIRECTION ( 'NONE',  ( -0.9730401042858035643, 0.2306359803922028717, 6.126766849694256332E-17 ) ) ;
#6081 = EDGE_CURVE ( 'NONE', #1184, #18635, #17035, .T. ) ;
#6082 = COORDINATED_UNIVERSAL_TIME_OFFSET ( 0, 0, .AHEAD. ) ;
#6083 = PRODUCT_DEFINITION_SHAPE ( 'NONE', 'NONE',  #23488 ) ;
#6084 = SECURITY_CLASSIFICATION ( '', '', #7266 ) ;
#6086 = EDGE_CURVE ( 'NONE', #17891, #19315, #22350, .T. ) ;
#6085 = ORIENTED_EDGE ( 'NONE', *, *, #20028, .T. ) ;
#6087 = VERTEX_POINT ( 'NONE', #5861 ) ;
#6088 = DIRECTION ( 'NONE',  ( 0.000000000000000000, -1.000000000000000000, 2.081668171172168119E-15 ) ) ;
#6089 = DIRECTION ( 'NONE',  ( -0.8823529412199648814, 0.4705882352125658197, 9.020562075079400046E-15 ) ) ;
#6090 = ORIENTED_EDGE ( 'NONE', *, *, #21436, .F. ) ;
#6091 = PERSON_AND_ORGANIZATION_ROLE ( 'classification_officer' ) ;
#6092 = CARTESIAN_POINT ( 'NONE',  ( 118.5079952955230027, -6.794810348829379620, -15.90000000000000036 ) ) ;
#6093 = CARTESIAN_POINT ( 'NONE',  ( 28.67817383939640052, -0.7594070262926470027, 11.00000000000019895 ) ) ;
#6094 = APPROVAL_ROLE ( '' ) ;
#6095 = DIRECTION ( 'NONE',  ( -0.9730401042858024541, 0.2306359803922080898, 5.959266323858942451E-17 ) ) ;
#6096 = CIRCLE ( 'NONE', #19369, 2.999999999999994227 ) ;
#6097 = CARTESIAN_POINT ( 'NONE',  ( 83.62762864230479920, -14.97056015138839946, -13.00000000000000000 ) ) ;
#6098 = CLOSED_SHELL ( 'NONE', ( #21423, #8761, #13358, #65, #18837, #12707, #14875, #246, #8064, #11318 ) ) ;
#6099 = FACE_OUTER_BOUND ( 'NONE', #17767, .T. ) ;
#6100 = SECURITY_CLASSIFICATION_LEVEL ( 'unclassified' ) ;
#6101 = CC_DESIGN_SECURITY_CLASSIFICATION ( #16700, ( #22008 ) ) ;
#6102 = CC_DESIGN_APPROVAL ( #3940, ( #7139 ) ) ;
#6103 = CARTESIAN_POINT ( 'NONE',  ( 114.1489752661110089, -25.18526831983109915, 3.000000000000000000 ) ) ;
#6104 = CARTESIAN_POINT ( 'NONE',  ( 31.11077410011089839, -1.335996977273150144, 11.00000000000019895 ) ) ;
#6105 = CC_DESIGN_DATE_AND_TIME_ASSIGNMENT ( #23062, #8244, ( #12089 ) ) ;
#6107 = CARTESIAN_POINT ( 'NONE',  ( 83.62762864230479920, -14.97056015138829821, 13.00000000000000000 ) ) ;
#6106 = AXIS2_PLACEMENT_3D ( 'NONE', #11521, #11861, #16943 ) ;
#6108 = DIRECTION ( 'NONE',  ( 0.9730401042858035643, -0.2306359803922028717, -5.958148513035547083E-17 ) ) ;
#6109 = DIRECTION ( 'NONE',  ( 9.248855984704951398E-11, -1.000000000000000000, 2.220446048198180498E-15 ) ) ;
#6110 = LINE ( 'NONE', #4559, #6924 ) ;
#6111 = AXIS2_PLACEMENT_3D ( 'NONE', #5754, #13012, #11005 ) ;
#6112 = ORIENTED_EDGE ( 'NONE', *, *, #529, .T. ) ;
#6113 = VERTEX_POINT ( 'NONE', #6220 ) ;
#6114 = CARTESIAN_POINT ( 'NONE',  ( -20.00000000397459843, 22.95208919256889857, -8.249999999995548450 ) ) ;
#6115 =( BOUNDED_CURVE ( )  B_SPLINE_CURVE ( 2, ( #22025, #11259, #14441 ),
 .UNSPECIFIED., .F., .F. ) 
 B_SPLINE_CURVE_WITH_KNOTS ( ( 3, 3 ),
 ( 0.000000000000000000, 0.08763271035584448143 ),
 .UNSPECIFIED. ) 
 CURVE ( )  GEOMETRIC_REPRESENTATION_ITEM ( )  RATIONAL_B_SPLINE_CURVE ( ( 1.000000000000000000, 1.077350269189626175, 1.077350269189624843 ) ) 
 REPRESENTATION_ITEM ( '' )  );
#6116 = DIRECTION ( 'NONE',  ( -0.005235963827110361700, 0.9999862922474493931, 0.000000000000000000 ) ) ;
#6117 = ORIENTED_EDGE ( 'NONE', *, *, #3383, .F. ) ;
#6118 = CARTESIAN_POINT ( 'NONE',  ( 39.27359436029389883, 22.26288585089439920, 12.99999999999970157 ) ) ;
#6119 = ORIENTED_EDGE ( 'NONE', *, *, #8601, .T. ) ;
#6120 = SECURITY_CLASSIFICATION ( '', '', #7934 ) ;
#6121 = CARTESIAN_POINT ( 'NONE',  ( 39.87324790931403840, 24.79279012203739541, 13.00000000000000000 ) ) ;
#6122 = LOCAL_TIME ( 14, 11, 27.00000000000000000, #21290 ) ;
#6123 = APPROVAL_ROLE ( '' ) ;
#6124 = CIRCLE ( 'NONE', #427, 2.750000000000002220 ) ;
#6125 = CARTESIAN_POINT ( 'NONE',  ( 0.000000000000000000, 0.000000000000000000, -5.000000000000000000 ) ) ;
#6126 = EDGE_CURVE ( 'NONE', #19134, #18417, #13463, .T. ) ;
#6127 = DATE_AND_TIME ( #6010, #14854 ) ;
#6128 = DIRECTION ( 'NONE',  ( 0.000000000000000000, 1.000000000000000000, 0.000000000000000000 ) ) ;
#6129 = CC_DESIGN_SECURITY_CLASSIFICATION ( #9926, ( #23490 ) ) ;
#6130 = DIRECTION ( 'NONE',  ( 6.281952996264450405E-17, 4.969341027148649850E-15, 1.000000000000000000 ) ) ;
#6131 = ORIENTED_EDGE ( 'NONE', *, *, #18854, .T. ) ;
#6132 = DIRECTION ( 'NONE',  ( -6.123230199561449365E-17, -4.868008300101910084E-15, -1.000000000000000000 ) ) ;
#6133 = ORIENTED_EDGE ( 'NONE', *, *, #14312, .F. ) ;
#6134 = CARTESIAN_POINT ( 'NONE',  ( 0.03403376487640599746, -6.499910899608420500, 8.873528816395729098E-14 ) ) ;
#6135 = PRODUCT_DEFINITION_FORMATION_WITH_SPECIFIED_SOURCE ( 'ANY', '', #10633, .NOT_KNOWN. ) ;
#6136 = CARTESIAN_POINT ( 'NONE',  ( 39.37089837072279863, 22.23982225285499936, -13.00000000000049916 ) ) ;
#6137 = ORIENTED_EDGE ( 'NONE', *, *, #13830, .T. ) ;
#6138 = DIRECTION ( 'NONE',  ( 0.9999862922474493931, 0.005235963827101436548, -1.466966272681988813E-16 ) ) ;
#6139 = AXIS2_PLACEMENT_3D ( 'NONE', #16695, #16354, #9350 ) ;
#6140 = CARTESIAN_POINT ( 'NONE',  ( -72.77122628570259621, -6.881121833202230142, 0.01852613985923039913 ) ) ;
#6141 = ORIENTED_EDGE ( 'NONE', *, *, #17700, .T. ) ;
#6142 = CALENDAR_DATE ( 2026, 31, 10 ) ;
#6143 = CARTESIAN_POINT ( 'NONE',  ( 12.60663921385023833, 13.09919299131893844, -3.665176466247191433E-15 ) ) ;
#6144 = CC_DESIGN_APPROVAL ( #6606, ( #1200 ) ) ;
#6145 = ORIENTED_EDGE ( 'NONE', *, *, #19519, .F. ) ;
#6146 = DATE_AND_TIME ( #13403, #16717 ) ;
#6147 = CYLINDRICAL_SURFACE ( 'NONE', #8050, 5.999999999999999112 ) ;
#6148 = ORIENTED_EDGE ( 'NONE', *, *, #6903, .T. ) ;
#6149 = EDGE_LOOP ( 'NONE', ( #12835, #9190, #2126, #22120 ) ) ;
#6150 = DIRECTION ( 'NONE',  ( -0.9730401042858035643, 0.2306359803922028717, 5.958148513035547083E-17 ) ) ;
#6151 = PERSON_AND_ORGANIZATION ( #11966, #8758 ) ;
#6152 = EDGE_CURVE ( 'NONE', #10876, #6317, #4429, .T. ) ;
#6153 = LOCAL_TIME ( 14, 11, 27.00000000000000000, #705 ) ;
#6154 = DATE_AND_TIME ( #8061, #5653 ) ;
#6155 = CARTESIAN_POINT ( 'NONE',  ( 118.6002496876800052, -6.405594307115060282, 15.90000000000000036 ) ) ;
#6156 = AXIS2_PLACEMENT_3D ( 'NONE', #18568, #20225, #13219 ) ;
#6157 = AXIS2_PLACEMENT_3D ( 'NONE', #11013, #18243, #14323 ) ;
#6158 = CC_DESIGN_DATE_AND_TIME_ASSIGNMENT ( #2103, #12917, ( #10735 ) ) ;
#6159 = AXIS2_PLACEMENT_3D ( 'NONE', #11289, #10611, #18518 ) ;
#6160 = APPROVAL_PERSON_ORGANIZATION ( #20509, #22683, #13272 ) ;
#6161 = DIRECTION ( 'NONE',  ( -2.982858504577240114E-17, 2.441916418604790135E-15, 1.000000000000000000 ) ) ;
#6162 = ORIENTED_EDGE ( 'NONE', *, *, #18536, .F. ) ;
#6163 = ADVANCED_FACE ( 'NONE', ( #18922 ), #2644, .F. ) ;
#6164 = ADVANCED_FACE ( 'NONE', ( #16775 ), #5970, .F. ) ;
#6165 = CIRCLE ( 'NONE', #12258, 1.250000000000000222 ) ;
#6166 = DATE_AND_TIME ( #927, #1143 ) ;
#6167 = EDGE_LOOP ( 'NONE', ( #5690, #1658, #6527, #14488 ) ) ;
#6168 = CIRCLE ( 'NONE', #9612, 3.499999999999998224 ) ;
#6169 = LINE ( 'NONE', #15415, #14464 ) ;
#6170 = DIRECTION ( 'NONE',  ( 0.9730401042858036753, -0.2306359803922031493, -5.959266323858673745E-17 ) ) ;
#6171 = ORIENTED_EDGE ( 'NONE', *, *, #18087, .F. ) ;
#6172 = ADVANCED_FACE ( 'NONE', ( #13227 ), #20460, .T. ) ;
#6173 = CC_DESIGN_APPROVAL ( #2995, ( #9978 ) ) ;
#6174 = DIRECTION ( 'NONE',  ( -7.840589463879458156E-32, 2.441916418604790135E-15, 1.000000000000000000 ) ) ;
#6175 = CARTESIAN_POINT ( 'NONE',  ( -31.64676348097539815, 7.334526001134540785, 2.500000000000000000 ) ) ;
#6176 = DIRECTION ( 'NONE',  ( 6.123230159571619958E-17, 0.000000000000000000, 1.000000000000000000 ) ) ;
#6177 = ORIENTED_EDGE ( 'NONE', *, *, #13473, .F. ) ;
#6178 = ORIENTED_EDGE ( 'NONE', *, *, #21107, .T. ) ;
#6179 = DIRECTION ( 'NONE',  ( 0.000000000000000000, 1.734723475976806848E-16, 1.000000000000000000 ) ) ;
#6180 = AXIS2_PLACEMENT_3D ( 'NONE', #8308, #4744, #21122 ) ;
#6181 = VERTEX_POINT ( 'NONE', #2421 ) ;
#6182 = AXIS2_PLACEMENT_3D ( 'NONE', #21876, #3487, #9306 ) ;
#6183 = CALENDAR_DATE ( 2026, 31, 10 ) ;
#6184 = ORIENTED_EDGE ( 'NONE', *, *, #18676, .F. ) ;
#6185 = TOROIDAL_SURFACE ( 'NONE', #17935, 3.750000000000000000, 0.5000000000000000000 ) ;
#6186 = ORIENTED_EDGE ( 'NONE', *, *, #7899, .T. ) ;
#6187 = CARTESIAN_POINT ( 'NONE',  ( -22.99995202268987171, -0.1204285676208978334, 9.211416015219178562E-14 ) ) ;
#6188 = APPROVAL_STATUS ( 'not_yet_approved' ) ;
#6189 = CARTESIAN_POINT ( 'NONE',  ( -20.00000000000000000, -20.00000000000000000, 8.000000000004559908 ) ) ;
#6190 = EDGE_CURVE ( 'NONE', #4103, #3305, #6813, .T. ) ;
#6191 = CARTESIAN_POINT ( 'NONE',  ( -20.00000000000000000, -20.00000000000000000, 0.000000000000000000 ) ) ;
#6192 = VECTOR ( 'NONE', #14657, 1000.000000000000000 ) ;
#6193 = AXIS2_PLACEMENT_3D ( 'NONE', #5925, #10829, #7251 ) ;
#6194 = CC_DESIGN_PERSON_AND_ORGANIZATION_ASSIGNMENT ( #12706, #16255, ( #9978 ) ) ;
#6195 = CC_DESIGN_APPROVAL ( #2102, ( #9078 ) ) ;
#6196 = APPROVAL ( #17697, 'UNSPECIFIED' ) ;
#6197 = DIRECTION ( 'NONE',  ( 1.000000000000000000, 0.000000000000000000, 0.000000000000000000 ) ) ;
#6198 = VECTOR ( 'NONE', #7320, 1000.000000000000000 ) ;
#6199 = EDGE_CURVE ( 'NONE', #11763, #11453, #2587, .T. ) ;
#6200 = CIRCLE ( 'NONE', #21369, 2.066999999999998394 ) ;
#6201 = EDGE_CURVE ( 'NONE', #554, #903, #1111, .T. ) ;
#6202 = CARTESIAN_POINT ( 'NONE',  ( 52.73786095581300515, -7.648876468381270222, -10.99076000000044928 ) ) ;
#6203 = PERSON_AND_ORGANIZATION ( #11966, #8758 ) ;
#6204 = CONICAL_SURFACE ( 'NONE', #5813, 2.283500000000000529, 0.7853981633974469467 ) ;
#6205 = APPROVAL ( #11849, 'UNSPECIFIED' ) ;
#6206 = ORIENTED_EDGE ( 'NONE', *, *, #21447, .F. ) ;
#6207 = FACE_OUTER_BOUND ( 'NONE', #11387, .T. ) ;
#6208 = DIRECTION ( 'NONE',  ( 0.000000000000000000, 0.000000000000000000, -1.000000000000000000 ) ) ;
#6209 = EDGE_LOOP ( 'NONE', ( #4923, #8151, #14860, #5385 ) ) ;
#6210 = CARTESIAN_POINT ( 'NONE',  ( -22.50000000000000000, -20.00000000000000000, 0.000000000000000000 ) ) ;
#6211 = CARTESIAN_POINT ( 'NONE',  ( -20.00000000000000000, -20.00000000000000000, 5.500000000004559020 ) ) ;
#6212 = ORIENTED_EDGE ( 'NONE', *, *, #13624, .T. ) ;
#6213 = VECTOR ( 'NONE', #18549, 1000.000000000000000 ) ;
#6214 = FACE_BOUND ( 'NONE', #3987, .T. ) ;
#6215 = CALENDAR_DATE ( 2026, 31, 10 ) ;
#6216 = AXIS2_PLACEMENT_3D ( 'NONE', #9238, #21922, #5654 ) ;
#6217 = ORIENTED_EDGE ( 'NONE', *, *, #7210, .T. ) ;
#6218 = ORIENTED_EDGE ( 'NONE', *, *, #3026, .F. ) ;
#6219 = PLANE ( 'NONE',  #21351 ) ;
#6220 = CARTESIAN_POINT ( 'NONE',  ( -9.489957111606940998, 28.27083100358139944, 2.500000000000000000 ) ) ;
#6221 = DIRECTION ( 'NONE',  ( -0.7071116276255479116, 0.000000000000000000, 0.7071019347143299161 ) ) ;
#6222 = AXIS2_PLACEMENT_3D ( 'NONE', #16728, #7382, #18539 ) ;
#6223 = DATE_AND_TIME ( #19167, #11841 ) ;
#6224 = DIRECTION ( 'NONE',  ( 0.9730401042858024541, -0.2306359803922080898, -5.959266323858942451E-17 ) ) ;
#6225 = ADVANCED_FACE ( 'NONE', ( #19505 ), #3019, .F. ) ;
#6226 = CARTESIAN_POINT ( 'NONE',  ( -2.499999999999973799, 4.120723506284736299E-15, 2.500000000000000000 ) ) ;
#6227 = SECURITY_CLASSIFICATION_LEVEL ( 'unclassified' ) ;
#6228 = DIRECTION ( 'NONE',  ( -0.1997366180463770735, -0.8426774492125654881, -0.4999999999999997780 ) ) ;
#6229 = ADVANCED_FACE ( 'NONE', ( #1323, #21271 ), #10612, .F. ) ;
#6230 = EDGE_CURVE ( 'NONE', #645, #8547, #10496, .T. ) ;
#6231 = DIRECTION ( 'NONE',  ( -0.02168293463503252055, 0.9997648975362223300, -2.428612866367530721E-15 ) ) ;
#6232 = COORDINATED_UNIVERSAL_TIME_OFFSET ( 0, 0, .AHEAD. ) ;
#6233 = VECTOR ( 'NONE', #19426, 1000.000000000000000 ) ;
#6234 = EDGE_CURVE ( 'NONE', #8780, #928, #1675, .T. ) ;
#6235 = DIRECTION ( 'NONE',  ( 0.000000000000000000, 0.000000000000000000, -1.000000000000000000 ) ) ;
#6236 = CIRCLE ( 'NONE', #2053, 3.499999999999996891 ) ;
#6237 = CARTESIAN_POINT ( 'NONE',  ( -60.02994014102380049, 8.478793778983318319, -5.000000000000000000 ) ) ;
#6238 = DIRECTION ( 'NONE',  ( 1.000000000000000000, 0.000000000000000000, 0.000000000000000000 ) ) ;
#6239 = FACE_OUTER_BOUND ( 'NONE', #9069, .T. ) ;
#6240 = DIRECTION ( 'NONE',  ( 3.211814849206744928E-17, -2.442368445299930605E-15, -1.000000000000000000 ) ) ;
#6241 = ORIENTED_EDGE ( 'NONE', *, *, #8628, .T. ) ;
#6242 = EDGE_LOOP ( 'NONE', ( #5652, #6186, #18069, #8899 ) ) ;
#6243 = PLANE ( 'NONE',  #3516 ) ;
#6244 = PLANE ( 'NONE',  #2232 ) ;
#6245 = EDGE_LOOP ( 'NONE', ( #20073, #9858 ) ) ;
#6246 = DIRECTION ( 'NONE',  ( -0.9730401042858035643, 0.2306359803922028717, 5.958148513035547083E-17 ) ) ;
#6247 = EDGE_LOOP ( 'NONE', ( #17779, #16109, #21613, #23021 ) ) ;
#6248 = FACE_OUTER_BOUND ( 'NONE', #21816, .T. ) ;
#6249 = APPROVAL_DATE_TIME ( #15139, #2102 ) ;
#6250 = PLANE ( 'NONE',  #3687 ) ;
#6251 = APPLICATION_CONTEXT ( 'configuration controlled 3d designs of mechanical parts and assemblies' ) ;
#6252 = EDGE_CURVE ( 'NONE', #11453, #23172, #19441, .T. ) ;
#6253 = CALENDAR_DATE ( 2026, 31, 10 ) ;
#6254 = SHAPE_REPRESENTATION_RELATIONSHIP ( 'NONE' , 'NONE' ,  #7037, #13910 ) ;
#6255 = DIRECTION ( 'NONE',  ( 0.1630842657209352065, 0.6880432561069602659, 0.7071067811865442421 ) ) ;
#6256 = CARTESIAN_POINT ( 'NONE',  ( 34.27523609350100031, 22.85428078671350249, -11.00000000000049916 ) ) ;
#6257 = ORIENTED_EDGE ( 'NONE', *, *, #5915, .T. ) ;
#6258 = LINE ( 'NONE', #13501, #13951 ) ;
#6259 = ADVANCED_BREP_SHAPE_REPRESENTATION ( '', ( #17099, #12739 ), #9323 ) ;
#6260 = VECTOR ( 'NONE', #5676, 1000.000000000000000 ) ;
#6261 = CARTESIAN_POINT ( 'NONE',  ( -25.01253141238650102, 26.70208918381559826, 5.500000000004510170 ) ) ;
#6262 = ORIENTED_EDGE ( 'NONE', *, *, #13132, .F. ) ;
#6263 =( BOUNDED_CURVE ( )  B_SPLINE_CURVE ( 2, ( #5246, #14735, #9287 ),
 .UNSPECIFIED., .F., .F. ) 
 B_SPLINE_CURVE_WITH_KNOTS ( ( 3, 3 ),
 ( 0.000000000000000000, 0.2336872276155859962 ),
 .UNSPECIFIED. ) 
 CURVE ( )  GEOMETRIC_REPRESENTATION_ITEM ( )  RATIONAL_B_SPLINE_CURVE ( ( 1.000000000000000000, 1.154700538379259900, 1.000000000000000000 ) ) 
 REPRESENTATION_ITEM ( '' )  );
#6264 = CARTESIAN_POINT ( 'NONE',  ( 11.50000000000000000, -23.36217782649110219, -2.500000000000000000 ) ) ;
#6265 = DIRECTION ( 'NONE',  ( -1.187319687680494078E-16, -2.805478249478345354E-20, -1.000000000000000000 ) ) ;
#6266 = UNCERTAINTY_MEASURE_WITH_UNIT (LENGTH_MEASURE( 1.000000000000000082E-05 ), #13093, 'distance_accuracy_value', 'NONE');
#6267 = EDGE_CURVE ( 'NONE', #16935, #8586, #18948, .T. ) ;
#6268 = CALENDAR_DATE ( 2026, 31, 10 ) ;
#6269 = FACE_OUTER_BOUND ( 'NONE', #18302, .T. ) ;
#6270 = ORIENTED_EDGE ( 'NONE', *, *, #10718, .T. ) ;
#6271 = DATE_TIME_ROLE ( 'classification_date' ) ;
#6272 = CARTESIAN_POINT ( 'NONE',  ( -32.65701080836369385, 9.273987487686079945, -3.750000000000000000 ) ) ;
#6273 = ORIENTED_EDGE ( 'NONE', *, *, #10184, .T. ) ;
#6274 = ORIENTED_EDGE ( 'NONE', *, *, #22263, .F. ) ;
#6275 = PERSON_AND_ORGANIZATION ( #11966, #8758 ) ;
#6276 = CIRCLE ( 'NONE', #8943, 2.500000000000000000 ) ;
#6277 = COORDINATED_UNIVERSAL_TIME_OFFSET ( 0, 0, .AHEAD. ) ;
#6278 = DIRECTION ( 'NONE',  ( -0.2306359803922076457, -0.9730401042858025651, 0.000000000000000000 ) ) ;
#6279 = CARTESIAN_POINT ( 'NONE',  ( 0.000000000000000000, 0.000000000000000000, -2.500000000000000000 ) ) ;
#6280 = ORIENTED_EDGE ( 'NONE', *, *, #1355, .T. ) ;
#6281 = CALENDAR_DATE ( 2026, 31, 10 ) ;
#6282 = PRODUCT_DEFINITION_SHAPE ( 'NONE', 'NONE',  #23495 ) ;
#6283 = ORIENTED_EDGE ( 'NONE', *, *, #5171, .T. ) ;
#6284 = DIRECTION ( 'NONE',  ( 0.000000000000000000, -1.000000000000000000, 2.081668171172169697E-15 ) ) ;
#6285 = DIRECTION ( 'NONE',  ( 0.000000000000000000, 4.336808689942006376E-14, 1.000000000000000000 ) ) ;
#6287 = ORIENTED_EDGE ( 'NONE', *, *, #4749, .T. ) ;
#6286 = EDGE_CURVE ( 'NONE', #11837, #255, #122, .T. ) ;
#6288 = ADVANCED_FACE ( 'NONE', ( #12283 ), #8229, .T. ) ;
#6289 = DIRECTION ( 'NONE',  ( -0.9730401042858023430, 0.2306359803922080620, 5.959266323858944916E-17 ) ) ;
#6290 = DIRECTION ( 'NONE',  ( -0.2306359803922053142, -0.9730401042858028982, 0.000000000000000000 ) ) ;
#6291 = DIRECTION ( 'NONE',  ( -0.9730401042858036753, 0.2306359803922028995, 5.958148513035547083E-17 ) ) ;
#6292 = ORIENTED_EDGE ( 'NONE', *, *, #13495, .T. ) ;
#6293 = ORIENTED_EDGE ( 'NONE', *, *, #18777, .T. ) ;
#6294 = DIRECTION ( 'NONE',  ( -0.2306359803922032603, -0.9730401042858034533, 0.000000000000000000 ) ) ;
#6295 = ORIENTED_EDGE ( 'NONE', *, *, #6003, .T. ) ;
#6296 = DATE_AND_TIME ( #18896, #15949 ) ;
#6297 = AXIS2_PLACEMENT_3D ( 'NONE', #3382, #12669, #16549 ) ;
#6298 = ORIENTED_EDGE ( 'NONE', *, *, #17317, .T. ) ;
#6299 = VERTEX_POINT ( 'NONE', #10260 ) ;
#6300 = FACE_OUTER_BOUND ( 'NONE', #21298, .T. ) ;
#6301 = APPROVAL_ROLE ( '' ) ;
#6302 = EDGE_CURVE ( 'NONE', #5211, #22277, #20246, .T. ) ;
#6303 = EDGE_CURVE ( 'NONE', #18306, #20086, #23267, .T. ) ;
#6304 = DIRECTION ( 'NONE',  ( -0.9730401042858035643, 0.2306359803922028717, -2.804983810440357322E-16 ) ) ;
#6305 = EDGE_CURVE ( 'NONE', #3952, #7758, #6934, .T. ) ;
#6306 =( GEOMETRIC_REPRESENTATION_CONTEXT ( 3 ) GLOBAL_UNCERTAINTY_ASSIGNED_CONTEXT ( ( #16296 ) ) GLOBAL_UNIT_ASSIGNED_CONTEXT ( ( #3501, #3264, #5058 ) ) REPRESENTATION_CONTEXT ( 'NONE', 'WORKASPACE' ) );
#6307 = CIRCLE ( 'NONE', #19585, 2.600000000000000089 ) ;
#6308 = DIRECTION ( 'NONE',  ( 0.2306359803922076457, 0.9730401042858023430, -1.412237191019970710E-17 ) ) ;
#6309 = PERSON_AND_ORGANIZATION ( #11966, #8758 ) ;
#6310 = ORIENTED_EDGE ( 'NONE', *, *, #18199, .F. ) ;
#6311 = FACE_OUTER_BOUND ( 'NONE', #1698, .T. ) ;
#6312 = DIRECTION ( 'NONE',  ( 0.000000000000000000, 0.000000000000000000, 1.000000000000000000 ) ) ;
#6313 = EDGE_LOOP ( 'NONE', ( #15568, #19995, #22501, #2766 ) ) ;
#6314 = ADVANCED_FACE ( 'NONE', ( #1437, #8702 ), #2883, .T. ) ;
#6315 = DIRECTION ( 'NONE',  ( -0.9730401042858035643, 0.2306359803922028717, 5.958148513035547083E-17 ) ) ;
#6316 = DIRECTION ( 'NONE',  ( 0.1153179901961009640, 0.4865200521429018377, 0.8660254037844385966 ) ) ;
#6317 = VERTEX_POINT ( 'NONE', #22938 ) ;
#6318 = CARTESIAN_POINT ( 'NONE',  ( -62.91331795724000386, 7.826945432762889787, 2.729132938682642617 ) ) ;
#6319 = CC_DESIGN_PERSON_AND_ORGANIZATION_ASSIGNMENT ( #22378, #14918, ( #5427 ) ) ;
#6320 = PERSON_AND_ORGANIZATION ( #11966, #8758 ) ;
#6321 = ORIENTED_EDGE ( 'NONE', *, *, #18467, .F. ) ;
#6322 = CC_DESIGN_PERSON_AND_ORGANIZATION_ASSIGNMENT ( #7236, #17926, ( #8400 ) ) ;
#6323 = ORIENTED_EDGE ( 'NONE', *, *, #22689, .F. ) ;
#6324 = LINE ( 'NONE', #17010, #19846 ) ;
#6325 = DIRECTION ( 'NONE',  ( 1.138590270679730064E-14, 2.220446049251240387E-15, 1.000000000000000000 ) ) ;
#6326 = VERTEX_POINT ( 'NONE', #19272 ) ;
#6327 = COORDINATED_UNIVERSAL_TIME_OFFSET ( 0, 0, .AHEAD. ) ;
#6328 = EDGE_CURVE ( 'NONE', #9834, #6033, #2991, .T. ) ;
#6329 = DIRECTION ( 'NONE',  ( -0.4188360644630711449, -0.9080618652410672453, 2.204917890671980836E-15 ) ) ;
#6330 = EDGE_CURVE ( 'NONE', #18371, #8501, #6691, .T. ) ;
#6331 = EDGE_CURVE ( 'NONE', #5079, #3196, #15252, .T. ) ;
#6332 = CARTESIAN_POINT ( 'NONE',  ( -0.5391976746803449627, 18.33937061236850141, -7.621247264287879719E-15 ) ) ;
#6333 = CONTEXT_DEPENDENT_SHAPE_REPRESENTATION ( #5210, #11414 ) ;
#6334 = EDGE_CURVE ( 'NONE', #8816, #3586, #8058, .T. ) ;
#6335 = CARTESIAN_POINT ( 'NONE',  ( -27.00000000000000000, -27.34999999999999787, 6.250000000000000000 ) ) ;
#6336 = VECTOR ( 'NONE', #20450, 1000.000000000000000 ) ;
#6337 = FACE_OUTER_BOUND ( 'NONE', #9256, .T. ) ;
#6338 = APPLICATION_PROTOCOL_DEFINITION ( 'international standard', 'config_control_design', 1994, #17938 ) ;
#6339 = AXIS2_PLACEMENT_3D ( 'NONE', #16677, #13031, #22379 ) ;
#6340 = AXIS2_PLACEMENT_3D ( 'NONE', #3599, #10869, #1800 ) ;
#6341 = DIRECTION ( 'NONE',  ( 0.9730401042858036753, -0.2306359803922028995, -5.432877459303547669E-17 ) ) ;
#6342 = LINE ( 'NONE', #4911, #21484 ) ;
#6343 = FACE_OUTER_BOUND ( 'NONE', #13109, .T. ) ;
#6344 = EDGE_CURVE ( 'NONE', #2592, #14730, #2803, .T. ) ;
#6345 = CARTESIAN_POINT ( 'NONE',  ( 41.15130700480209924, 11.54075009235119964, -15.50000000000000000 ) ) ;
#6346 = AXIS2_PLACEMENT_3D ( 'NONE', #18822, #10266, #22478 ) ;
#6347 = CARTESIAN_POINT ( 'NONE',  ( 28.89837840081079889, -1.998294948772289858, -13.00000000000039968 ) ) ;
#6348 = CYLINDRICAL_SURFACE ( 'NONE', #5396, 0.3999999999999982458 ) ;
#6349 = VERTEX_POINT ( 'NONE', #12733 ) ;
#6350 = ORIENTED_EDGE ( 'NONE', *, *, #4750, .T. ) ;
#6351 = CARTESIAN_POINT ( 'NONE',  ( 39.27359436029429673, 22.26288585089420025, -13.00000000000049916 ) ) ;
#6352 = FACE_OUTER_BOUND ( 'NONE', #223, .T. ) ;
#6353 = VECTOR ( 'NONE', #16152, 1000.000000000000000 ) ;
#6354 = ORIENTED_EDGE ( 'NONE', *, *, #15483, .T. ) ;
#6355 = EDGE_CURVE ( 'NONE', #1257, #14820, #9283, .T. ) ;
#6356 = DIRECTION ( 'NONE',  ( 0.8846153846153629319, -0.4663213712685850276, 0.000000000000000000 ) ) ;
#6357 = EDGE_CURVE ( 'NONE', #19233, #4824, #9046, .T. ) ;
#6358 = AXIS2_PLACEMENT_3D ( 'NONE', #20977, #22975, #17661 ) ;
#6359 = EDGE_LOOP ( 'NONE', ( #6941, #21906 ) ) ;
#6360 = AXIS2_PLACEMENT_3D ( 'NONE', #17492, #6228, #20815 ) ;
#6361 = CARTESIAN_POINT ( 'NONE',  ( 58.73439644601031517, 17.65016624305016890, -15.00924000000053660 ) ) ;
#6362 = AXIS2_PLACEMENT_3D ( 'NONE', #245, #14750, #21977 ) ;
#6363 = PERSON_AND_ORGANIZATION ( #11966, #8758 ) ;
#6364 = CARTESIAN_POINT ( 'NONE',  ( 43.66832999130209458, 21.22121844545429781, 13.00000000000000000 ) ) ;
#6365 = APPROVAL_ROLE ( '' ) ;
#6366 = DIRECTION ( 'NONE',  ( -0.6880432561069586006, 0.1630842657209346236, 0.7071067811865459074 ) ) ;
#6367 = CARTESIAN_POINT ( 'NONE',  ( 43.45766680872284837, 21.27115113520779843, -13.00000000000030020 ) ) ;
#6368 = CIRCLE ( 'NONE', #11329, 3.499999999999999556 ) ;
#6369 = CARTESIAN_POINT ( 'NONE',  ( 37.27955344062029752, 9.375336445360778370, 27.68999999999999773 ) ) ;
#6370 = ORIENTED_EDGE ( 'NONE', *, *, #7221, .F. ) ;
#6371 = DIRECTION ( 'NONE',  ( -8.911056267098788616E-18, -1.998401444326210262E-15, -1.000000000000000000 ) ) ;
#6372 = VECTOR ( 'NONE', #15837, 1000.000000000000000 ) ;
#6373 = EDGE_CURVE ( 'NONE', #3684, #10212, #16278, .T. ) ;
#6374 = CARTESIAN_POINT ( 'NONE',  ( -1.540112692620030144, -27.34999999999999787, 5.000000000000000000 ) ) ;
#6375 = AXIS2_PLACEMENT_3D ( 'NONE', #2921, #12326, #4935 ) ;
#6376 = ORIENTED_EDGE ( 'NONE', *, *, #850, .T. ) ;
#6377 = LINE ( 'NONE', #16942, #14659 ) ;
#6378 = FACE_BOUND ( 'NONE', #19961, .T. ) ;
#6379 = COORDINATED_UNIVERSAL_TIME_OFFSET ( 0, 0, .AHEAD. ) ;
#6380 = CARTESIAN_POINT ( 'NONE',  ( -19.49999999982519938, -0.1021026942257689946, 3.750000000000000000 ) ) ;
#6381 = EDGE_CURVE ( 'NONE', #5291, #17008, #121, .T. ) ;
#6382 = ORIENTED_EDGE ( 'NONE', *, *, #23303, .T. ) ;
#6383 = ORIENTED_EDGE ( 'NONE', *, *, #12770, .F. ) ;
#6384 = ADVANCED_FACE ( 'NONE', ( #7270, #17967 ), #12623, .T. ) ;
#6385 = APPLICATION_PROTOCOL_DEFINITION ( 'international standard', 'config_control_design', 1994, #16400 ) ;
#6386 = CYLINDRICAL_SURFACE ( 'NONE', #10356, 3.999999999999998668 ) ;
#6387 = ORIENTED_EDGE ( 'NONE', *, *, #3065, .T. ) ;
#6388 = DIRECTION ( 'NONE',  ( 0.000000000000000000, -1.000000000000000000, 0.000000000000000000 ) ) ;
#6389 = AXIS2_PLACEMENT_3D ( 'NONE', #10303, #17415, #15747 ) ;
#6390 = COORDINATED_UNIVERSAL_TIME_OFFSET ( 0, 0, .AHEAD. ) ;
#6391 = PERSON_AND_ORGANIZATION_ROLE ( 'classification_officer' ) ;
#6392 = AXIS2_PLACEMENT_3D ( 'NONE', #14274, #12397, #23409 ) ;
#6393 = CARTESIAN_POINT ( 'NONE',  ( 35.94015251278350576, 11.23436983788223209, 27.55602540378454179 ) ) ;
#6394 = CARTESIAN_POINT ( 'NONE',  ( -19.99975861755300244, 22.95209442650120124, 2.499999999999900524 ) ) ;
#6395 = ORIENTED_EDGE ( 'NONE', *, *, #1567, .T. ) ;
#6396 = DATE_TIME_ROLE ( 'creation_date' ) ;
#6397 = ORIENTED_EDGE ( 'NONE', *, *, #22919, .T. ) ;
#6398 = CARTESIAN_POINT ( 'NONE',  ( 32.67740532107718820, -5.566061131680290153, -13.00000000000039968 ) ) ;
#6399 = CARTESIAN_POINT ( 'NONE',  ( -56.98461483124570037, -21.79876819407909849, -1.072991366992009803E-14 ) ) ;
#6400 = ORIENTED_EDGE ( 'NONE', *, *, #21166, .T. ) ;
#6401 = APPROVAL ( #11087, 'UNSPECIFIED' ) ;
#6402 = CARTESIAN_POINT ( 'NONE',  ( -25.29411765129259848, 25.77561860384869874, 6.750000000004519940 ) ) ;
#6403 = CLOSED_SHELL ( 'NONE', ( #10600, #6056, #16190, #1733, #5992, #3396 ) ) ;
#6405 = CIRCLE ( 'NONE', #11688, 8.250000000000003553 ) ;
#6404 = CARTESIAN_POINT ( 'NONE',  ( 28.67817383939640052, -0.7594070262926470027, 11.00000000000019895 ) ) ;
#6406 = DIRECTION ( 'NONE',  ( -0.6862566701892842680, -0.7273594590164591533, 3.576853004787541598E-15 ) ) ;
#6407 = ORIENTED_EDGE ( 'NONE', *, *, #21724, .T. ) ;
#6408 = ORIENTED_EDGE ( 'NONE', *, *, #20418, .F. ) ;
#6409 = DIRECTION ( 'NONE',  ( -0.7071067811865475727, 0.000000000000000000, -0.7071067811865475727 ) ) ;
#6410 = VERTEX_POINT ( 'NONE', #7394 ) ;
#6411 = PERSON_AND_ORGANIZATION ( #11966, #8758 ) ;
#6412 = ORIENTED_EDGE ( 'NONE', *, *, #4774, .T. ) ;
#6413 = ORIENTED_EDGE ( 'NONE', *, *, #499, .F. ) ;
#6414 = CARTESIAN_POINT ( 'NONE',  ( -62.91331795724000386, 7.826945432762889787, 2.150173005478499992E-15 ) ) ;
#6415 = APPLICATION_PROTOCOL_DEFINITION ( 'international standard', 'config_control_design', 1994, #13089 ) ;
#6416 = DIRECTION ( 'NONE',  ( 0.000000000000000000, 0.5102823824563427202, -0.8600069128528436968 ) ) ;
#6417 = EDGE_CURVE ( 'NONE', #16220, #20341, #19119, .T. ) ;
#6418 =( REPRESENTATION_RELATIONSHIP ('NONE','NONE', #19303, #15060 ) REPRESENTATION_RELATIONSHIP_WITH_TRANSFORMATION ( #5896 )SHAPE_REPRESENTATION_RELATIONSHIP( ) );
#6419 = CARTESIAN_POINT ( 'NONE',  ( 118.5079952955230027, -6.794810348829359192, -15.50000000000000000 ) ) ;
#6420 = DATE_AND_TIME ( #13449, #1177 ) ;
#6421 = PRODUCT_DEFINITION_SHAPE ( 'NONE', 'NONE',  #16907 ) ;
#6422 = ORIENTED_EDGE ( 'NONE', *, *, #20454, .T. ) ;
#6423 = SECURITY_CLASSIFICATION ( '', '', #6227 ) ;
#6424 = LINE ( 'NONE', #15339, #23147 ) ;
#6425 = AXIS2_PLACEMENT_3D ( 'NONE', #853, #17376, #19616 ) ;
#6426 = DIRECTION ( 'NONE',  ( 5.964507377817298878E-17, 4.861311874385510251E-15, 1.000000000000000000 ) ) ;
#6427 = ORIENTED_EDGE ( 'NONE', *, *, #5645, .T. ) ;
#6428 = ADVANCED_FACE ( 'NONE', ( #7048, #7158 ), #12953, .T. ) ;
#6429 = DIRECTION ( 'NONE',  ( 0.000000000000000000, 1.000000000000000000, 0.000000000000000000 ) ) ;
#6430 = CARTESIAN_POINT ( 'NONE',  ( -16.50082286259691955, 23.02797946379192950, -5.000000000000060396 ) ) ;
#6431 = ORIENTED_EDGE ( 'NONE', *, *, #4204, .F. ) ;
#6432 = DIRECTION ( 'NONE',  ( -2.982858504577314686E-17, 2.441916418604790135E-15, 1.000000000000000000 ) ) ;
#6433 = PERSON_AND_ORGANIZATION ( #11966, #8758 ) ;
#6434 = EDGE_CURVE ( 'NONE', #1138, #12006, #16508, .T. ) ;
#6435 = ORIENTED_EDGE ( 'NONE', *, *, #8520, .F. ) ;
#6436 = ORIENTED_EDGE ( 'NONE', *, *, #7237, .T. ) ;
#6437 = FACE_OUTER_BOUND ( 'NONE', #4981, .T. ) ;
#6438 = DIRECTION ( 'NONE',  ( -0.005235963827101452160, 0.9999862922474493931, 5.492442074325202057E-16 ) ) ;
#6439 = ORIENTED_EDGE ( 'NONE', *, *, #7656, .F. ) ;
#6440 = MECHANICAL_CONTEXT ( 'NONE', #22918, 'mechanical' ) ;
#6441 = LINE ( 'NONE', #12051, #9237 ) ;
#6442 = DIRECTION ( 'NONE',  ( -0.9730401042858036753, 0.2306359803922031493, 5.432877459303543355E-17 ) ) ;
#6443 = CIRCLE ( 'NONE', #20478, 0.2000000000000016209 ) ;
#6444 = DIRECTION ( 'NONE',  ( 0.000000000000000000, 0.000000000000000000, -1.000000000000000000 ) ) ;
#6445 = EDGE_CURVE ( 'NONE', #2018, #7239, #8117, .T. ) ;
#6446 = AXIS2_PLACEMENT_3D ( 'NONE', #17629, #6704, #4910 ) ;
#6447 = APPROVAL ( #7765, 'UNKNOWN' ) ;
#6448 = DIRECTION ( 'NONE',  ( -0.9730401042858024541, 0.2306359803922080898, 5.959266323858942451E-17 ) ) ;
#6449 = APPROVAL_STATUS ( 'not_yet_approved' ) ;
#6450 = APPROVAL ( #856, 'UNSPECIFIED' ) ;
#6451 = CARTESIAN_POINT ( 'NONE',  ( 36.19076168202141019, 7.791205907825823118, 8.820012287919203331 ) ) ;
#6452 = DIRECTION ( 'NONE',  ( -0.2306359803922009288, -0.9730401042858040084, 0.000000000000000000 ) ) ;
#6453 = ADVANCED_FACE ( 'NONE', ( #10966 ), #18185, .T. ) ;
#6454 = ADVANCED_FACE ( 'NONE', ( #5588 ), #8885, .F. ) ;
#6455 = PLANE ( 'NONE',  #17710 ) ;
#6456 = LOCAL_TIME ( 14, 11, 27.00000000000000000, #22768 ) ;
#6457 = CARTESIAN_POINT ( 'NONE',  ( 28.89837840081079889, -1.998294948772169954, 13.00000000000019895 ) ) ;
#6458 = PLANE ( 'NONE',  #3495 ) ;
#6459 = AXIS2_PLACEMENT_3D ( 'NONE', #10892, #17764, #14202 ) ;
#6460 = DIRECTION ( 'NONE',  ( 0.9730401042858036753, -0.2306359803922031493, -5.432877459303553216E-17 ) ) ;
#6461 = CIRCLE ( 'NONE', #16272, 3.499999999999998668 ) ;
#6462 = ORIENTED_EDGE ( 'NONE', *, *, #801, .F. ) ;
#6463 = ORIENTED_EDGE ( 'NONE', *, *, #980, .T. ) ;
#6464 = CARTESIAN_POINT ( 'NONE',  ( 121.3909450504253584, 5.368190954742481757, -13.00000000000000000 ) ) ;
#6465 = CARTESIAN_POINT ( 'NONE',  ( -30.72441677844230057, -6.660963241697680282, 5.500000000000089706 ) ) ;
#6466 = ORIENTED_EDGE ( 'NONE', *, *, #13044, .F. ) ;
#6467 = AXIS2_PLACEMENT_3D ( 'NONE', #17823, #2215, #423 ) ;
#6468 = CARTESIAN_POINT ( 'NONE',  ( 37.10730959030829723, 23.96304573415820016, 11.00000000000000000 ) ) ;
#6469 = ORIENTED_EDGE ( 'NONE', *, *, #21724, .F. ) ;
#6470 = CARTESIAN_POINT ( 'NONE',  ( 117.1011158151309957, -12.73035498497280038, -19.59999999999999787 ) ) ;
#6471 = VECTOR ( 'NONE', #19278, 1000.000000000000000 ) ;
#6472 = COORDINATED_UNIVERSAL_TIME_OFFSET ( 0, 0, .AHEAD. ) ;
#6473 = CARTESIAN_POINT ( 'NONE',  ( -25.29411765129399825, 25.77561860384869874, -5.499999999994369837 ) ) ;
#6474 = ADVANCED_FACE ( 'NONE', ( #3796 ), #229, .T. ) ;
#6475 = PRODUCT_DEFINITION_SHAPE ( 'NONE', 'NONE',  #20819 ) ;
#6476 = APPROVAL_PERSON_ORGANIZATION ( #4286, #7938, #14843 ) ;
#6477 = DATE_AND_TIME ( #19422, #14871 ) ;
#6478 =( LENGTH_UNIT ( ) NAMED_UNIT ( * ) SI_UNIT ( .MILLI., .METRE. ) );
#6479 = APPROVAL_PERSON_ORGANIZATION ( #17783, #11587, #57 ) ;
#6480 = CYLINDRICAL_SURFACE ( 'NONE', #3526, 0.3999999999999982458 ) ;
#6481 = PRODUCT_RELATED_PRODUCT_CATEGORY ( 'detail', '', ( #576 ) ) ;
#6482 = DIRECTION ( 'NONE',  ( -3.210834492181045054E-17, 2.441916418604790135E-15, 1.000000000000000000 ) ) ;
#6483 = APPROVAL ( #18158, 'UNSPECIFIED' ) ;
#6484 = CARTESIAN_POINT ( 'NONE',  ( 2.664535259100379799E-14, -1.554450629062440126E-15, 5.000000000000000000 ) ) ;
#6485 = ORIENTED_EDGE ( 'NONE', *, *, #249, .F. ) ;
#6487 = AXIS2_PLACEMENT_3D ( 'NONE', #17663, #3275, #1364 ) ;
#6486 = FACE_OUTER_BOUND ( 'NONE', #4311, .T. ) ;
#6488 = EDGE_CURVE ( 'NONE', #10685, #9733, #5771, .T. ) ;
#6489 = EDGE_CURVE ( 'NONE', #1396, #2445, #11105, .T. ) ;
#6490 = CARTESIAN_POINT ( 'NONE',  ( -20.00000000397270128, 22.95208919257159863, 5.000000000004460432 ) ) ;
#6491 = EDGE_LOOP ( 'NONE', ( #9619, #22336, #18153, #15288 ) ) ;
#6492 = CARTESIAN_POINT ( 'NONE',  ( -23.50000000000000000, -20.00000000000000000, 2.500000000000000000 ) ) ;
#6493 = DIRECTION ( 'NONE',  ( 0.9949874374308178560, 0.09999999677427207079, -1.144917494144692682E-14 ) ) ;
#6494 = CC_DESIGN_SECURITY_CLASSIFICATION ( #12572, ( #6875 ) ) ;
#6495 = CONTEXT_DEPENDENT_SHAPE_REPRESENTATION ( #17357, #14989 ) ;
#6496 = CARTESIAN_POINT ( 'NONE',  ( 34.82690584700060299, 8.415117834048050582, 29.25000000000000000 ) ) ;
#6497 = CC_DESIGN_APPROVAL ( #12792, ( #12089 ) ) ;
#6498 = EDGE_LOOP ( 'NONE', ( #20289, #6653, #5268, #315, #4016 ) ) ;
#6499 = VERTEX_POINT ( 'NONE', #9515 ) ;
#6500 = APPROVAL_ROLE ( '' ) ;
#6501 = CARTESIAN_POINT ( 'NONE',  ( 45.41807264205800010, 29.54199202163849947, 9.133960000000000079 ) ) ;
#6502 = ORIENTED_EDGE ( 'NONE', *, *, #2083, .T. ) ;
#6503 = APPROVAL_PERSON_ORGANIZATION ( #15759, #13695, #19557 ) ;
#6504 = DIRECTION ( 'NONE',  ( 1.000000000000000000, 3.099353312215988811E-62, 0.000000000000000000 ) ) ;
#6505 = ORGANIZATION ( 'NAUO-ORG21', 'UNSPECIFIED', 'UNSPECIFIED' ) ;
#6506 = APPROVAL_STATUS ( 'not_yet_approved' ) ;
#6507 = ADVANCED_FACE ( 'NONE', ( #6300 ), #4645, .T. ) ;
#6508 = CALENDAR_DATE ( 2026, 31, 10 ) ;
#6509 = DIRECTION ( 'NONE',  ( 0.000000000000000000, 0.000000000000000000, 1.000000000000000000 ) ) ;
#6510 = LOCAL_TIME ( 14, 11, 27.00000000000000000, #15400 ) ;
#6511 = CARTESIAN_POINT ( 'NONE',  ( -30.72441677844230057, -6.660963241697680282, 3.000000000000090150 ) ) ;
#6512 = CIRCLE ( 'NONE', #19789, 4.250000000000001776 ) ;
#6513 = ORIENTED_EDGE ( 'NONE', *, *, #11158, .F. ) ;
#6514 = ADVANCED_FACE ( 'NONE', ( #7970 ), #18792, .F. ) ;
#6515 = CIRCLE ( 'NONE', #2720, 2.500000000000000444 ) ;
#6516 = MECHANICAL_CONTEXT ( 'NONE', #17171, 'mechanical' ) ;
#6517 = EDGE_CURVE ( 'NONE', #23382, #22935, #17595, .T. ) ;
#6518 = VERTEX_POINT ( 'NONE', #5836 ) ;
#6519 = APPROVAL_PERSON_ORGANIZATION ( #9715, #10821, #2458 ) ;
#6520 = DIRECTION ( 'NONE',  ( 0.9949874374308235181, 0.09999999677421511635, -1.179611963664228193E-14 ) ) ;
#6521 = CARTESIAN_POINT ( 'NONE',  ( 52.73786095581300515, -7.648876468381139659, 10.99076000000024855 ) ) ;
#6522 = VERTEX_POINT ( 'NONE', #20550 ) ;
#6523 = DIRECTION ( 'NONE',  ( 0.9730401042858035643, -0.2306359803922028717, -5.432877459303547053E-17 ) ) ;
#6524 = DIRECTION ( 'NONE',  ( -0.2306359803922094498, -0.9730401042858020100, 1.412237191019847142E-17 ) ) ;
#6525 = CARTESIAN_POINT ( 'NONE',  ( 58.25686728443110241, 17.76335315678750248, 13.00000000000000000 ) ) ;
#6526 = VERTEX_POINT ( 'NONE', #20436 ) ;
#6527 = ORIENTED_EDGE ( 'NONE', *, *, #4762, .T. ) ;
#6528 = DIRECTION ( 'NONE',  ( 4.028143194477080210E-16, 2.054129435991050111E-15, 1.000000000000000000 ) ) ;
#6529 = ORIENTED_EDGE ( 'NONE', *, *, #2107, .F. ) ;
#6530 = SECURITY_CLASSIFICATION_LEVEL ( 'unclassified' ) ;
#6531 = LOCAL_TIME ( 14, 11, 27.00000000000000000, #15433 ) ;
#6532 = ORIENTED_EDGE ( 'NONE', *, *, #4848, .T. ) ;
#6533 = ORIENTED_EDGE ( 'NONE', *, *, #8370, .F. ) ;
#6534 = CARTESIAN_POINT ( 'NONE',  ( -16.50082286259682363, 23.02797946379152094, -2.500000000000039968 ) ) ;
#6535 = MECHANICAL_CONTEXT ( 'NONE', #7911, 'mechanical' ) ;
#6536 = AXIS2_PLACEMENT_3D ( 'NONE', #9299, #7409, #19986 ) ;
#6537 = PERSON ( 'NAUO-PER38', 'UNSPECIFIED', 'UNSPECIFIED', ('UNSPECIFIED'), ('UNSPECIFIED'), ('UNSPECIFIED') ) ;
#6538 = VECTOR ( 'NONE', #2586, 1000.000000000000000 ) ;
#6539 = AXIS2_PLACEMENT_3D ( 'NONE', #16164, #562, #18400 ) ;
#6540 = DIRECTION ( 'NONE',  ( 1.138590270679730064E-14, 2.220446049251240387E-15, 1.000000000000000000 ) ) ;
#6541 =( BOUNDED_CURVE ( )  B_SPLINE_CURVE ( 2, ( #13741, #5074, #23220 ),
 .UNSPECIFIED., .F., .F. ) 
 B_SPLINE_CURVE_WITH_KNOTS ( ( 3, 3 ),
 ( 0.000000000000000000, 0.08763271035584378754 ),
 .UNSPECIFIED. ) 
 CURVE ( )  GEOMETRIC_REPRESENTATION_ITEM ( )  RATIONAL_B_SPLINE_CURVE ( ( 1.000000000000000000, 1.077350269189625731, 1.077350269189625065 ) ) 
 REPRESENTATION_ITEM ( '' )  );
#6542 = ORGANIZATION ( 'NAUO-ORG33', 'UNSPECIFIED', 'UNSPECIFIED' ) ;
#6543 = APPROVAL ( #2512, 'UNSPECIFIED' ) ;
#6544 = AXIS2_PLACEMENT_3D ( 'NONE', #5006, #10490, #20916 ) ;
#6545 = EDGE_CURVE ( 'NONE', #12545, #3638, #22450, .T. ) ;
#6546 = VECTOR ( 'NONE', #15553, 999.9999999999998863 ) ;
#6547 =( NAMED_UNIT ( * ) SI_UNIT ( $, .STERADIAN. ) SOLID_ANGLE_UNIT ( ) );
#6548 = CARTESIAN_POINT ( 'NONE',  ( -29.94163891957289891, 6.343422587376370103, 2.500000000000000000 ) ) ;
#6549 = PLANE ( 'NONE',  #13986 ) ;
#6550 = DATE_AND_TIME ( #22565, #20526 ) ;
#6551 = SECURITY_CLASSIFICATION ( '', '', #18875 ) ;
#6552 = EDGE_LOOP ( 'NONE', ( #173, #4123, #18368, #22368 ) ) ;
#6553 = FACE_OUTER_BOUND ( 'NONE', #21581, .T. ) ;
#6554 = AXIS2_PLACEMENT_3D ( 'NONE', #6211, #365, #22110 ) ;
#6555 = DIRECTION ( 'NONE',  ( 2.269881297312570136E-47, 1.000000000000000000, -2.269881297312570136E-47 ) ) ;
#6556 = ORIENTED_EDGE ( 'NONE', *, *, #545, .F. ) ;
#6557 = CIRCLE ( 'NONE', #1605, 2.749999999999999112 ) ;
#6558 = PERSON ( 'NAUO-PER2', 'UNSPECIFIED', 'UNSPECIFIED', ('UNSPECIFIED'), ('UNSPECIFIED'), ('UNSPECIFIED') ) ;
#6559 = CARTESIAN_POINT ( 'NONE',  ( 0.000000000000000000, -1.554450629062379975E-15, 5.000000000000000000 ) ) ;
#6560 = VECTOR ( 'NONE', #7906, 1000.000000000000000 ) ;
#6561 = DIRECTION ( 'NONE',  ( 0.000000000000000000, 0.000000000000000000, -1.000000000000000000 ) ) ;
#6562 = DIRECTION ( 'NONE',  ( 0.000000000000000000, -1.000000000000000000, 1.011971878839179923E-16 ) ) ;
#6563 = VERTEX_POINT ( 'NONE', #9764 ) ;
#6564 = DIRECTION ( 'NONE',  ( -0.9730401042858022320, 0.2306359803922080343, 5.959266323858941219E-17 ) ) ;
#6565 = APPLICATION_CONTEXT ( 'configuration controlled 3d designs of mechanical parts and assemblies' ) ;
#6566 = VECTOR ( 'NONE', #9927, 1000.000000000000114 ) ;
#6567 = PERSON_AND_ORGANIZATION_ROLE ( 'creator' ) ;
#6568 = ADVANCED_FACE ( 'NONE', ( #16616 ), #17154, .F. ) ;
#6569 = ORIENTED_EDGE ( 'NONE', *, *, #13866, .F. ) ;
#6570 = ORIENTED_EDGE ( 'NONE', *, *, #6190, .F. ) ;
#6571 = CARTESIAN_POINT ( 'NONE',  ( -27.00000000000000000, -20.00000000000000000, -5.000000000000000000 ) ) ;
#6572 = CARTESIAN_POINT ( 'NONE',  ( 36.30836311812279860, 20.59233593730780143, -13.00000000000049916 ) ) ;
#6573 = AXIS2_PLACEMENT_3D ( 'NONE', #8273, #1121, #15856 ) ;
#6574 = VERTEX_POINT ( 'NONE', #18434 ) ;
#6575 = PERSON_AND_ORGANIZATION_ROLE ( 'classification_officer' ) ;
#6576 = CIRCLE ( 'NONE', #19835, 2.500000000000000000 ) ;
#6577 = LINE ( 'NONE', #17843, #3905 ) ;
#6578 = CC_DESIGN_APPROVAL ( #947, ( #4302 ) ) ;
#6579 = DIRECTION ( 'NONE',  ( 0.000000000000000000, 0.000000000000000000, 1.000000000000000000 ) ) ;
#6580 = PERSON_AND_ORGANIZATION ( #5122, #4523 ) ;
#6581 = CIRCLE ( 'NONE', #1622, 2.500000000000001776 ) ;
#6582 = DIRECTION ( 'NONE',  ( 0.9730401042858036753, -0.2306359803922028995, -5.432877459303547669E-17 ) ) ;
#6583 = AXIS2_PLACEMENT_3D ( 'NONE', #4427, #22226, #16773 ) ;
#6584 = AXIS2_PLACEMENT_3D ( 'NONE', #1702, #12530, #3962 ) ;
#6585 =( NAMED_UNIT ( * ) SI_UNIT ( $, .STERADIAN. ) SOLID_ANGLE_UNIT ( ) );
#6586 = DIRECTION ( 'NONE',  ( 0.000000000000000000, 0.000000000000000000, -1.000000000000000000 ) ) ;
#6587 = PERSON_AND_ORGANIZATION ( #11966, #8758 ) ;
#6588 = FACE_OUTER_BOUND ( 'NONE', #21477, .T. ) ;
#6589 = CIRCLE ( 'NONE', #22491, 2.499999999999998668 ) ;
#6590 = CARTESIAN_POINT ( 'NONE',  ( -27.00000000000000000, -20.00000000000000000, 2.500000000000000000 ) ) ;
#6591 = CARTESIAN_POINT ( 'NONE',  ( 27.73073027566755044, -1.721531772301079899, -13.00000000000000000 ) ) ;
#6592 = LOCAL_TIME ( 14, 11, 27.00000000000000000, #16539 ) ;
#6593 = CIRCLE ( 'NONE', #15690, 4.750000000000001776 ) ;
#6594 = FACE_BOUND ( 'NONE', #20717, .T. ) ;
#6595 = DIRECTION ( 'NONE',  ( 6.123237831918399306E-17, -1.569224110909209817E-30, -1.000000000000000000 ) ) ;
#6596 = ORIENTED_EDGE ( 'NONE', *, *, #17781, .F. ) ;
#6597 = AXIS2_PLACEMENT_3D ( 'NONE', #15571, #635, #8461 ) ;
#6598 = CARTESIAN_POINT ( 'NONE',  ( -20.00000000000000000, -20.00000000000000000, -2.500000000000000000 ) ) ;
#6599 = ORIENTED_EDGE ( 'NONE', *, *, #6600, .F. ) ;
#6600 = EDGE_CURVE ( 'NONE', #668, #3168, #7677, .T. ) ;
#6601 = AXIS2_PLACEMENT_3D ( 'NONE', #10444, #1607, #4950 ) ;
#6602 = ORIENTED_EDGE ( 'NONE', *, *, #14795, .T. ) ;
#6603 = DIRECTION ( 'NONE',  ( -0.1153179901961009640, -0.4865200521429018377, -0.8660254037844385966 ) ) ;
#6604 = CARTESIAN_POINT ( 'NONE',  ( -32.42721070416779838, 10.33414378941739997, -3.750000000000000000 ) ) ;
#6605 = VERTEX_POINT ( 'NONE', #11563 ) ;
#6606 = APPROVAL ( #8618, 'UNKNOWN' ) ;
#6607 = CARTESIAN_POINT ( 'NONE',  ( 28.94448933012489888, 0.3641629059906499877, -13.00000000000039968 ) ) ;
#6608 = ORIENTED_EDGE ( 'NONE', *, *, #14740, .F. ) ;
#6609 = DIRECTION ( 'NONE',  ( 0.8846153846153640421, -0.4663213712685829182, 0.000000000000000000 ) ) ;
#6610 = APPROVAL_STATUS ( 'not_yet_approved' ) ;
#6611 = CARTESIAN_POINT ( 'NONE',  ( 35.84667945578129888, -10.83917230622230043, 3.100000000000039613 ) ) ;
#6612 = EDGE_CURVE ( 'NONE', #1782, #18157, #13539, .T. ) ;
#6613 = EDGE_CURVE ( 'NONE', #14262, #23458, #2621, .T. ) ;
#6614 = VECTOR ( 'NONE', #3847, 1000.000000000000114 ) ;
#6615 = PERSON_AND_ORGANIZATION ( #7388, #2346 ) ;
#6616 = CIRCLE ( 'NONE', #19883, 2.066999999999999726 ) ;
#6617 = DIRECTION ( 'NONE',  ( 0.2306359803922020946, 0.9730401042858036753, -4.006172263299086280E-15 ) ) ;
#6618 = DIRECTION ( 'NONE',  ( 0.000000000000000000, -5.527220191599521464E-16, 1.000000000000000000 ) ) ;
#6619 =( LENGTH_UNIT ( ) NAMED_UNIT ( * ) SI_UNIT ( .MILLI., .METRE. ) );
#6620 = DIRECTION ( 'NONE',  ( -6.662161563160872600E-09, 1.000000000000000000, -1.982541115402066096E-15 ) ) ;
#6621 = VERTEX_POINT ( 'NONE', #9399 ) ;
#6622 = CARTESIAN_POINT ( 'NONE',  ( -28.45655959278310121, -6.649088660734180145, -0.7325259402522680263 ) ) ;
#6623 = DESIGN_CONTEXT ( 'detailed design', #14278, 'design' ) ;
#6624 = DIRECTION ( 'NONE',  ( 3.211814849206744928E-17, -2.442368445299930605E-15, -1.000000000000000000 ) ) ;
#6625 = VERTEX_POINT ( 'NONE', #6187 ) ;
#6626 = CARTESIAN_POINT ( 'NONE',  ( 33.53206126189282088, 9.578550183514808580, -8.976164948525093834 ) ) ;
#6627 = LINE ( 'NONE', #19318, #12976 ) ;
#6628 = EDGE_CURVE ( 'NONE', #18216, #21775, #3177, .T. ) ;
#6629 = APPROVAL_DATE_TIME ( #2585, #12836 ) ;
#6630 = FACE_OUTER_BOUND ( 'NONE', #14986, .T. ) ;
#6631 = ORIENTED_EDGE ( 'NONE', *, *, #21080, .T. ) ;
#6632 = ORIENTED_EDGE ( 'NONE', *, *, #14216, .F. ) ;
#6634 = PERSON_AND_ORGANIZATION ( #11966, #8758 ) ;
#6633 = CC_DESIGN_PERSON_AND_ORGANIZATION_ASSIGNMENT ( #5298, #14222, ( #2395 ) ) ;
#6635 = DIRECTION ( 'NONE',  ( 0.2306359803922080343, 0.9730401042858022320, -1.412237191019910313E-17 ) ) ;
#6636 = ORIENTED_EDGE ( 'NONE', *, *, #7362, .F. ) ;
#6637 = PRODUCT_DEFINITION ( 'UNKNOWN', '', #16369, #14206 ) ;
#6638 = CARTESIAN_POINT ( 'NONE',  ( 52.93501234483849771, 21.14904221214005631, -13.00000000000000000 ) ) ;
#6639 = CALENDAR_DATE ( 2026, 31, 10 ) ;
#6640 = EDGE_CURVE ( 'NONE', #15872, #22384, #18900, .T. ) ;
#6641 = EDGE_CURVE ( 'NONE', #14346, #300, #17103, .T. ) ;
#6642 = PRODUCT_DEFINITION_SHAPE ( 'NONE', 'NONE',  #1591 ) ;
#6643 = CC_DESIGN_PERSON_AND_ORGANIZATION_ASSIGNMENT ( #18778, #8300, ( #9386 ) ) ;
#6644 = APPROVAL_STATUS ( 'not_yet_approved' ) ;
#6645 = CARTESIAN_POINT ( 'NONE',  ( -20.00479999606179859, 1.846597379377909798, -5.499999999995520028 ) ) ;
#6646 = EDGE_CURVE ( 'NONE', #551, #16156, #7733, .T. ) ;
#6647 = DIRECTION ( 'NONE',  ( -0.9730401042858022320, 0.2306359803922080343, 5.959266323858941219E-17 ) ) ;
#6648 = ORIENTED_EDGE ( 'NONE', *, *, #17255, .F. ) ;
#6649 = AXIS2_PLACEMENT_3D ( 'NONE', #8410, #17207, #2706 ) ;
#6650 = ORIENTED_EDGE ( 'NONE', *, *, #2235, .F. ) ;
#6651 = DIRECTION ( 'NONE',  ( -8.623081276789554834E-17, -1.054188326053478339E-16, -1.000000000000000000 ) ) ;
#6652 = DIRECTION ( 'NONE',  ( 0.1153179901961009640, 0.4865200521429018377, -0.8660254037844385966 ) ) ;
#6653 = ORIENTED_EDGE ( 'NONE', *, *, #2892, .T. ) ;
#6654 = EDGE_CURVE ( 'NONE', #19958, #22663, #19485, .T. ) ;
#6655 = DIRECTION ( 'NONE',  ( -2.982858504577314686E-17, 2.441916418604790135E-15, 1.000000000000000000 ) ) ;
#6656 = DIRECTION ( 'NONE',  ( 0.7806762821592939661, -0.6249356306644249237, -1.759009604640482141E-13 ) ) ;
#6657 = DIRECTION ( 'NONE',  ( 1.000000000000000000, 0.000000000000000000, 0.000000000000000000 ) ) ;
#6658 = ORIENTED_EDGE ( 'NONE', *, *, #18798, .F. ) ;
#6659 = EDGE_LOOP ( 'NONE', ( #5205, #12488, #21879, #8966, #12043 ) ) ;
#6660 = CARTESIAN_POINT ( 'NONE',  ( -17.54011269262000283, -27.34999999999999787, -2.500000000000000000 ) ) ;
#6661 = ORIENTED_EDGE ( 'NONE', *, *, #10889, .T. ) ;
#6662 = PERSON_AND_ORGANIZATION ( #11966, #8758 ) ;
#6663 = ORIENTED_EDGE ( 'NONE', *, *, #17682, .F. ) ;
#6664 = CIRCLE ( 'NONE', #5124, 2.499999999999999112 ) ;
#6665 = ORIENTED_EDGE ( 'NONE', *, *, #19947, .F. ) ;
#6666 = CARTESIAN_POINT ( 'NONE',  ( 26.57755037370653639, -6.586732293730098498, -13.00000000000000000 ) ) ;
#6667 = CALENDAR_DATE ( 2026, 31, 10 ) ;
#6668 = EDGE_CURVE ( 'NONE', #4824, #6526, #9242, .T. ) ;
#6669 = EDGE_CURVE ( 'NONE', #3862, #3011, #9744, .T. ) ;
#6670 = DIRECTION ( 'NONE',  ( -0.005235963827101452160, 0.9999862922474493931, 5.492442074325202057E-16 ) ) ;
#6671 =( NAMED_UNIT ( * ) PLANE_ANGLE_UNIT ( ) SI_UNIT ( $, .RADIAN. ) );
#6672 = DIRECTION ( 'NONE',  ( -0.9730401042858022320, 0.2306359803922080343, 5.959266323858941219E-17 ) ) ;
#6673 = CARTESIAN_POINT ( 'NONE',  ( 52.26033179423370001, -7.535689554643850485, 13.00000000000019895 ) ) ;
#6674 = PERSON_AND_ORGANIZATION ( #11966, #8758 ) ;
#6675 = AXIS2_PLACEMENT_3D ( 'NONE', #3405, #8763, #3533 ) ;
#6676 = ORIENTED_EDGE ( 'NONE', *, *, #7975, .F. ) ;
#6677 = CARTESIAN_POINT ( 'NONE',  ( -18.05391955182270181, 22.49081825942809942, -2.500000000000000000 ) ) ;
#6678 = DIRECTION ( 'NONE',  ( -0.9730401042858036753, 0.2306359803922028995, 5.959266323858677443E-17 ) ) ;
#6679 = ORIENTED_EDGE ( 'NONE', *, *, #21355, .T. ) ;
#6680 = CIRCLE ( 'NONE', #10485, 6.000000000000000000 ) ;
#6681 = CARTESIAN_POINT ( 'NONE',  ( -20.00000000397270128, 22.95208919256889857, 4.454121720691780225E-12 ) ) ;
#6682 = LINE ( 'NONE', #11364, #15693 ) ;
#6683 = FACE_OUTER_BOUND ( 'NONE', #4188, .T. ) ;
#6684 = ORIENTED_EDGE ( 'NONE', *, *, #14741, .T. ) ;
#6685 = CARTESIAN_POINT ( 'NONE',  ( 113.2033677465029911, -29.17473274740279976, 3.100000000000039613 ) ) ;
#6686 = SECURITY_CLASSIFICATION_LEVEL ( 'unclassified' ) ;
#6687 = PRODUCT_DEFINITION_SHAPE ( 'NONE', 'NONE',  #23513 ) ;
#6688 = ORIENTED_EDGE ( 'NONE', *, *, #13414, .F. ) ;
#6689 = ORIENTED_EDGE ( 'NONE', *, *, #1509, .F. ) ;
#6690 = DIRECTION ( 'NONE',  ( 0.2306359803922080620, 0.9730401042858023430, -5.935311836577789915E-15 ) ) ;
#6691 = LINE ( 'NONE', #13924, #22069 ) ;
#6692 = EDGE_CURVE ( 'NONE', #8196, #19011, #15202, .T. ) ;
#6693 = CARTESIAN_POINT ( 'NONE',  ( 39.37089837072289811, 22.23982225285509884, 13.00000000000000000 ) ) ;
#6694 = PERSON_AND_ORGANIZATION ( #11966, #8758 ) ;
#6695 = EDGE_CURVE ( 'NONE', #22846, #11102, #943, .T. ) ;
#6696 = DIRECTION ( 'NONE',  ( 0.5021071549687922131, -0.8648054144888001060, 0.000000000000000000 ) ) ;
#6697 = CARTESIAN_POINT ( 'NONE',  ( 37.48968750243700043, 22.68571848161329996, 11.84529946162074943 ) ) ;
#6698 = DIRECTION ( 'NONE',  ( -9.248903203239929993E-11, 1.000000000000000000, -2.220446028257650359E-15 ) ) ;
#6699 = AXIS2_PLACEMENT_3D ( 'NONE', #15437, #22674, #6416 ) ;
#6700 =( LENGTH_UNIT ( ) NAMED_UNIT ( * ) SI_UNIT ( .MILLI., .METRE. ) );
#6701 = VERTEX_POINT ( 'NONE', #15684 ) ;
#6702 = CARTESIAN_POINT ( 'NONE',  ( 2.664535259100379799E-14, -1.554450629062440126E-15, 2.500000000000000000 ) ) ;
#6703 = CALENDAR_DATE ( 2026, 31, 10 ) ;
#6704 = DIRECTION ( 'NONE',  ( -0.9730401042858024541, 0.2306359803922080898, 5.959266323858942451E-17 ) ) ;
#6705 = CARTESIAN_POINT ( 'NONE',  ( -16.00004797695773107, -0.08377682083104374955, 9.108728376131438406E-14 ) ) ;
#6706 = APPLICATION_CONTEXT ( 'configuration controlled 3d designs of mechanical parts and assemblies' ) ;
#6707 = CARTESIAN_POINT ( 'NONE',  ( 36.09092202081949807, 8.115512906978469942, 29.25000000000000000 ) ) ;
#6708 = CIRCLE ( 'NONE', #17708, 4.250000000000000000 ) ;
#6709 = FACE_OUTER_BOUND ( 'NONE', #2761, .T. ) ;
#6710 = VECTOR ( 'NONE', #5718, 1000.000000000000114 ) ;
#6711 = LINE ( 'NONE', #8252, #14106 ) ;
#6712 = ORIENTED_EDGE ( 'NONE', *, *, #17655, .T. ) ;
#6713 = DIRECTION ( 'NONE',  ( 0.005235963827108352890, -0.9999862922474493931, -2.671135040551771006E-18 ) ) ;
#6714 = ORIENTED_EDGE ( 'NONE', *, *, #19359, .F. ) ;
#6715 = ORIENTED_EDGE ( 'NONE', *, *, #4612, .T. ) ;
#6716 = CARTESIAN_POINT ( 'NONE',  ( 37.10730959030829723, 23.96304573415810069, -11.00000000000049916 ) ) ;
#6717 = CARTESIAN_POINT ( 'NONE',  ( 5.000000000000000000, -28.60000000000000142, -21.50000000000000000 ) ) ;
#6718 = ORIENTED_EDGE ( 'NONE', *, *, #684, .F. ) ;
#6719 = CARTESIAN_POINT ( 'NONE',  ( 36.17078849317570644, 12.20740994216802910, 19.99999999999998934 ) ) ;
#6720 = VERTEX_POINT ( 'NONE', #3084 ) ;
#6721 = DIRECTION ( 'NONE',  ( 0.2306359803921919083, 0.9730401042858062288, 8.673617379884073337E-14 ) ) ;
#6722 = PERSON_AND_ORGANIZATION_ROLE ( 'design_owner' ) ;
#6723 = CARTESIAN_POINT ( 'NONE',  ( 35.54906454756380185, 11.32706792491969772, 27.55602540378455600 ) ) ;
#6724 = CIRCLE ( 'NONE', #11280, 2.749999999999999112 ) ;
#6725 = CALENDAR_DATE ( 2026, 31, 10 ) ;
#6726 = AXIS2_PLACEMENT_3D ( 'NONE', #9418, #20885, #805 ) ;
#6727 = CIRCLE ( 'NONE', #23375, 2.499999999999999556 ) ;
#6728 = ADVANCED_FACE ( 'NONE', ( #21026 ), #3207, .T. ) ;
#6729 = DIRECTION ( 'NONE',  ( -0.2306359803921919083, -0.9730401042858062288, 0.000000000000000000 ) ) ;
#6730 = EDGE_CURVE ( 'NONE', #7581, #15508, #22840, .T. ) ;
#6731 = DIRECTION ( 'NONE',  ( 0.9730401042858036753, -0.2306359803922031493, -5.432877459303553216E-17 ) ) ;
#6732 = CARTESIAN_POINT ( 'NONE',  ( 0.000000000000000000, 0.000000000000000000, 0.000000000000000000 ) ) ;
#6733 = DIRECTION ( 'NONE',  ( -0.9730401042858035643, 0.2306359803922028717, 5.959266323858679908E-17 ) ) ;
#6734 = ORIENTED_EDGE ( 'NONE', *, *, #7042, .T. ) ;
#6735 = DIRECTION ( 'NONE',  ( 2.269747459788990007E-13, 2.220446049250330436E-15, 1.000000000000000000 ) ) ;
#6736 = DIRECTION ( 'NONE',  ( -0.2306359803922028995, -0.9730401042858036753, 1.343075398093749487E-16 ) ) ;
#6737 = VERTEX_POINT ( 'NONE', #19012 ) ;
#6738 = AXIS2_PLACEMENT_3D ( 'NONE', #18202, #12518, #12855 ) ;
#6739 = CARTESIAN_POINT ( 'NONE',  ( -20.00000000000000000, -25.00000000000000000, -5.499999999995458744 ) ) ;
#6740 = DIRECTION ( 'NONE',  ( 0.2306359803922076457, 0.9730401042858025651, 0.000000000000000000 ) ) ;
#6741 = EDGE_CURVE ( 'NONE', #20016, #9507, #10352, .T. ) ;
#6742 = ADVANCED_FACE ( 'NONE', ( #17592 ), #17241, .F. ) ;
#6743 = VERTEX_POINT ( 'NONE', #1409 ) ;
#6744 = VECTOR ( 'NONE', #1353, 1000.000000000000114 ) ;
#6745 = FACE_OUTER_BOUND ( 'NONE', #7904, .T. ) ;
#6746 = ORIENTED_EDGE ( 'NONE', *, *, #5020, .T. ) ;
#6747 = ORIENTED_EDGE ( 'NONE', *, *, #22321, .T. ) ;
#6748 = PERSON_AND_ORGANIZATION_ROLE ( 'creator' ) ;
#6749 = CARTESIAN_POINT ( 'NONE',  ( -24.50000000000000000, -30.47499999999999787, 21.50000000000000000 ) ) ;
#6750 = ORIENTED_EDGE ( 'NONE', *, *, #16840, .T. ) ;
#6751 = CARTESIAN_POINT ( 'NONE',  ( 33.87576285740820481, 21.16892588828840260, -13.00000000000049916 ) ) ;
#6752 =( REPRESENTATION_RELATIONSHIP ('NONE','NONE', #18121, #1735 ) REPRESENTATION_RELATIONSHIP_WITH_TRANSFORMATION ( #15528 )SHAPE_REPRESENTATION_RELATIONSHIP( ) );
#6753 = SHAPE_DEFINITION_REPRESENTATION ( #15381, #11141 ) ;
#6754 = COORDINATED_UNIVERSAL_TIME_OFFSET ( 0, 0, .AHEAD. ) ;
#6755 = CIRCLE ( 'NONE', #12814, 2.066999999999999726 ) ;
#6756 = CARTESIAN_POINT ( 'NONE',  ( 43.84419854219520829, 0.000000000000000000, -65.86501949894326913 ) ) ;
#6757 = CIRCLE ( 'NONE', #20017, 4.999999999999995559 ) ;
#6758 = ADVANCED_FACE ( 'NONE', ( #10116 ), #10230, .T. ) ;
#6759 = AXIS2_PLACEMENT_3D ( 'NONE', #22867, #10189, #9950 ) ;
#6760 = LINE ( 'NONE', #21108, #18336 ) ;
#6761 = ORIENTED_EDGE ( 'NONE', *, *, #5645, .F. ) ;
#6762 = APPROVAL ( #3965, 'UNKNOWN' ) ;
#6763 = PRODUCT_DEFINITION ( 'UNKNOWN', '', #795, #21787 ) ;
#6764 = VERTEX_POINT ( 'NONE', #6666 ) ;
#6765 = CIRCLE ( 'NONE', #22654, 2.066999999999999726 ) ;
#6766 = LINE ( 'NONE', #21466, #3475 ) ;
#6767 = DIRECTION ( 'NONE',  ( 0.000000000000000000, -1.000000000000000000, 1.534091707905539548E-92 ) ) ;
#6768 = ORIENTED_EDGE ( 'NONE', *, *, #10780, .T. ) ;
#6769 = ADVANCED_FACE ( 'NONE', ( #13657 ), #12020, .F. ) ;
#6770 = ADVANCED_FACE ( 'NONE', ( #4637 ), #19240, .T. ) ;
#6771 = CARTESIAN_POINT ( 'NONE',  ( 32.79777292954499757, -5.491820719290930519, -13.00000000000039968 ) ) ;
#6772 = DIRECTION ( 'NONE',  ( -0.9997651245102240347, -0.02167246670447264822, 0.000000000000000000 ) ) ;
#6773 = CIRCLE ( 'NONE', #14335, 2.066999999999999726 ) ;
#6774 = ORIENTED_EDGE ( 'NONE', *, *, #14739, .F. ) ;
#6775 = ORIENTED_EDGE ( 'NONE', *, *, #11244, .T. ) ;
#6776 = DIRECTION ( 'NONE',  ( 0.000000000000000000, 0.000000000000000000, -1.000000000000000000 ) ) ;
#6777 = EDGE_LOOP ( 'NONE', ( #20427, #3428, #1404, #14691, #15263, #11336 ) ) ;
#6778 = COORDINATED_UNIVERSAL_TIME_OFFSET ( 0, 0, .AHEAD. ) ;
#6779 = ORIENTED_EDGE ( 'NONE', *, *, #6417, .F. ) ;
#6780 = ORIENTED_EDGE ( 'NONE', *, *, #22866, .T. ) ;
#6781 = CARTESIAN_POINT ( 'NONE',  ( 34.14207834813680620, 22.29249582057189727, 15.00000000000000000 ) ) ;
#6782 = CIRCLE ( 'NONE', #4492, 2.066999999999999726 ) ;
#6783 = APPROVAL_STATUS ( 'not_yet_approved' ) ;
#6784 = LINE ( 'NONE', #14010, #1362 ) ;
#6785 = EDGE_CURVE ( 'NONE', #18892, #19958, #21242, .T. ) ;
#6786 = CARTESIAN_POINT ( 'NONE',  ( -16.50058068176714343, 23.02794805996801841, 3.749999999999949818 ) ) ;
#6787 = CALENDAR_DATE ( 2026, 31, 10 ) ;
#6788 = VECTOR ( 'NONE', #15562, 1000.000000000000227 ) ;
#6789 = VERTEX_POINT ( 'NONE', #6534 ) ;
#6790 = LINE ( 'NONE', #12030, #1521 ) ;
#6791 = DIRECTION ( 'NONE',  ( 6.124378941434239724E-17, -2.274246353359159970E-33, 1.000000000000000000 ) ) ;
#6792 = ORIENTED_EDGE ( 'NONE', *, *, #14829, .T. ) ;
#6793 = ADVANCED_FACE ( 'NONE', ( #11913 ), #21721, .F. ) ;
#6794 = EDGE_CURVE ( 'NONE', #5829, #4745, #12260, .T. ) ;
#6795 = CYLINDRICAL_SURFACE ( 'NONE', #13189, 2.499999999999998668 ) ;
#6796 = FACE_OUTER_BOUND ( 'NONE', #13869, .T. ) ;
#6797 = CYLINDRICAL_SURFACE ( 'NONE', #21711, 2.458500000000000352 ) ;
#6798 = VERTEX_POINT ( 'NONE', #2967 ) ;
#6799 = CARTESIAN_POINT ( 'NONE',  ( 5.000000000000000000, -27.34999999999999787, -6.250000000000000000 ) ) ;
#6800 = APPLICATION_PROTOCOL_DEFINITION ( 'international standard', 'config_control_design', 1994, #3800 ) ;
#6801 = ORIENTED_EDGE ( 'NONE', *, *, #5492, .F. ) ;
#6802 = ORIENTED_EDGE ( 'NONE', *, *, #14162, .T. ) ;
#6803 = DIRECTION ( 'NONE',  ( 2.269747459788994803E-13, 2.220446049250470459E-15, 1.000000000000000000 ) ) ;
#6804 = DIRECTION ( 'NONE',  ( 1.213490492418603984E-15, 4.861311874477930828E-15, 1.000000000000000000 ) ) ;
#6805 = FACE_BOUND ( 'NONE', #4364, .T. ) ;
#6806 = DATE_AND_TIME ( #1440, #441 ) ;
#6807 = CARTESIAN_POINT ( 'NONE',  ( -22.99999999999959854, -19.33065833018789803, 25.00000000000000000 ) ) ;
#6808 = CARTESIAN_POINT ( 'NONE',  ( 38.63934541421534163, 19.58702556410841922, 12.99999999999970512 ) ) ;
#6809 = CARTESIAN_POINT ( 'NONE',  ( 114.8178196092480050, -22.36345201740219935, -20.00000000000000000 ) ) ;
#6810 = ADVANCED_FACE ( 'NONE', ( #13897 ), #11783, .F. ) ;
#6811 = DIRECTION ( 'NONE',  ( 1.000000000000000000, 0.000000000000000000, 0.000000000000000000 ) ) ;
#6812 = SECURITY_CLASSIFICATION ( '', '', #9979 ) ;
#6813 = CIRCLE ( 'NONE', #6425, 2.499999999999998668 ) ;
#6814 = VERTEX_POINT ( 'NONE', #8316 ) ;
#6815 = FACE_OUTER_BOUND ( 'NONE', #4075, .T. ) ;
#6816 = APPROVAL_DATE_TIME ( #21410, #2625 ) ;
#6817 = CARTESIAN_POINT ( 'NONE',  ( 37.41678276236235234, 8.790432847337626754, 8.984918777770046106 ) ) ;
#6818 = DIRECTION ( 'NONE',  ( -0.2306359803922080620, -0.9730401042858023430, -3.574477303645826527E-15 ) ) ;
#6819 = EDGE_CURVE ( 'NONE', #16084, #11146, #1300, .T. ) ;
#6820 = CARTESIAN_POINT ( 'NONE',  ( -20.00000000397270128, 22.95208919256889857, -5.499999999995559996 ) ) ;
#6821 = CARTESIAN_POINT ( 'NONE',  ( -20.00000000397469790, 22.95208919256889857, -8.499999999995548450 ) ) ;
#6822 = ADVANCED_FACE ( 'NONE', ( #23023 ), #22789, .F. ) ;
#6823 = CARTESIAN_POINT ( 'NONE',  ( -12.59661859123050043, -1.225550774622850225, -6.749999999997189803 ) ) ;
#6824 = ORIENTED_EDGE ( 'NONE', *, *, #16581, .F. ) ;
#6825 = PLANE ( 'NONE',  #11891 ) ;
#6826 = UNCERTAINTY_MEASURE_WITH_UNIT (LENGTH_MEASURE( 1.000000000000000082E-05 ), #13320, 'distance_accuracy_value', 'NONE');
#6827 = PRODUCT_DEFINITION_SHAPE ( 'NONE', 'NONE',  #18531 ) ;
#6828 = VERTEX_POINT ( 'NONE', #1754 ) ;
#6829 = DIRECTION ( 'NONE',  ( -0.005235963827121941846, 0.9999862922474492821, 7.400535959148351896E-19 ) ) ;
#6830 = DIRECTION ( 'NONE',  ( -0.2306359803922031770, -0.9730401042858035643, 1.407521210652529060E-17 ) ) ;
#6831 = AXIS2_PLACEMENT_3D ( 'NONE', #23405, #17977, #3119 ) ;
#6832 = ORIENTED_EDGE ( 'NONE', *, *, #3441, .T. ) ;
#6833 = VECTOR ( 'NONE', #16978, 999.9999999999998863 ) ;
#6834 = LINE ( 'NONE', #1232, #11138 ) ;
#6835 = ORIENTED_EDGE ( 'NONE', *, *, #21686, .T. ) ;
#6836 = LINE ( 'NONE', #1351, #18962 ) ;
#6837 = CALENDAR_DATE ( 2026, 31, 10 ) ;
#6838 = DIRECTION ( 'NONE',  ( -0.9080618652418041004, 0.4188360644614733674, -1.040834085574019418E-15 ) ) ;
#6839 = CARTESIAN_POINT ( 'NONE',  ( 27.87922736721089834, -4.130116823142910398, 13.00000000000019895 ) ) ;
#6840 = PRODUCT_DEFINITION ( 'UNKNOWN', '', #796, #9424 ) ;
#6841 = DIRECTION ( 'NONE',  ( -0.005235963827101446956, 0.9999862922474495042, 5.492442074325198113E-16 ) ) ;
#6842 = DIRECTION ( 'NONE',  ( 1.000000000000000000, 0.000000000000000000, 0.000000000000000000 ) ) ;
#6843 = SECURITY_CLASSIFICATION ( '', '', #2237 ) ;
#6844 = AXIS2_PLACEMENT_3D ( 'NONE', #16208, #6977, #14421 ) ;
#6845 = DIRECTION ( 'NONE',  ( -0.9730401042858024541, 0.2306359803922080898, 5.959266323858942451E-17 ) ) ;
#6846 = VECTOR ( 'NONE', #22909, 1000.000000000000227 ) ;
#6847 = ORIENTED_EDGE ( 'NONE', *, *, #8696, .T. ) ;
#6848 = FACE_OUTER_BOUND ( 'NONE', #1424, .T. ) ;
#6849 = DESIGN_CONTEXT ( 'detailed design', #18712, 'design' ) ;
#6850 = CARTESIAN_POINT ( 'NONE',  ( 34.14207834813680620, 22.29249582057189727, 15.00000000000000000 ) ) ;
#6851 = ORIENTED_EDGE ( 'NONE', *, *, #14300, .T. ) ;
#6852 = LINE ( 'NONE', #14085, #21482 ) ;
#6853 = FACE_OUTER_BOUND ( 'NONE', #4252, .T. ) ;
#6854 = AXIS2_PLACEMENT_3D ( 'NONE', #7984, #11575, #9888 ) ;
#6855 = ORIENTED_EDGE ( 'NONE', *, *, #19571, .F. ) ;
#6856 = CALENDAR_DATE ( 2026, 31, 10 ) ;
#6857 = CARTESIAN_POINT ( 'NONE',  ( -58.40964484538829993, -25.30627767975780174, -2.500000000000000000 ) ) ;
#6858 = AXIS2_PLACEMENT_3D ( 'NONE', #5947, #11439, #13207 ) ;
#6859 = VERTEX_POINT ( 'NONE', #19588 ) ;
#6860 = ORIENTED_EDGE ( 'NONE', *, *, #6695, .F. ) ;
#6861 = PERSON_AND_ORGANIZATION ( #11966, #8758 ) ;
#6862 = LINE ( 'NONE', #6749, #3866 ) ;
#6863 = ADVANCED_FACE ( 'NONE', ( #16137 ), #14476, .F. ) ;
#6864 = EDGE_LOOP ( 'NONE', ( #4321, #15777 ) ) ;
#6865 = CC_DESIGN_APPROVAL ( #21563, ( #14054 ) ) ;
#6866 = DIRECTION ( 'NONE',  ( -4.028143194477080210E-16, -2.054129435991050111E-15, -1.000000000000000000 ) ) ;
#6867 = APPROVAL_PERSON_ORGANIZATION ( #7756, #5175, #11585 ) ;
#6868 = PERSON_AND_ORGANIZATION ( #11966, #8758 ) ;
#6869 = CONTEXT_DEPENDENT_SHAPE_REPRESENTATION ( #7953, #16679 ) ;
#6870 = FACE_OUTER_BOUND ( 'NONE', #23428, .T. ) ;
#6871 = AXIS2_PLACEMENT_3D ( 'NONE', #22162, #17950, #19600 ) ;
#6872 = DIRECTION ( 'NONE',  ( 2.979184080115845427E-09, -0.4472135954999635343, -0.8944271909999130798 ) ) ;
#6873 = ORIENTED_EDGE ( 'NONE', *, *, #14491, .T. ) ;
#6874 = CLOSED_SHELL ( 'NONE', ( #1778, #2343, #3296, #6229, #18004, #20671 ) ) ;
#6875 = PRODUCT_DEFINITION_FORMATION_WITH_SPECIFIED_SOURCE ( 'ANY', '', #4919, .NOT_KNOWN. ) ;
#6876 = ORIENTED_EDGE ( 'NONE', *, *, #14220, .T. ) ;
#6877 = CC_DESIGN_APPROVAL ( #2625, ( #796 ) ) ;
#6878 = DIRECTION ( 'NONE',  ( -0.9999862922474491711, -0.005235963827128302210, 1.239088197126291310E-16 ) ) ;
#6879 = CARTESIAN_POINT ( 'NONE',  ( -1.276518118481687392, 16.16736622398676460, -1.549884229762907576E-17 ) ) ;
#6880 = ORIENTED_EDGE ( 'NONE', *, *, #1144, .F. ) ;
#6881 = CIRCLE ( 'NONE', #15971, 5.000000000000002665 ) ;
#6882 = CC_DESIGN_SECURITY_CLASSIFICATION ( #1162, ( #23513 ) ) ;
#6883 = CARTESIAN_POINT ( 'NONE',  ( 122.7747609327790030, 11.20643158045800014, 9.133960000000000079 ) ) ;
#6884 = DIRECTION ( 'NONE',  ( 0.000000000000000000, 0.000000000000000000, 1.000000000000000000 ) ) ;
#6885 = VERTEX_POINT ( 'NONE', #19702 ) ;
#6886 = ORGANIZATION ( 'NAUO-ORG17', 'UNSPECIFIED', 'UNSPECIFIED' ) ;
#6887 = ORIENTED_EDGE ( 'NONE', *, *, #14065, .F. ) ;
#6888 = ORIENTED_EDGE ( 'NONE', *, *, #1340, .F. ) ;
#6889 = VECTOR ( 'NONE', #6736, 999.9999999999998863 ) ;
#6890 = PERSON_AND_ORGANIZATION ( #11966, #8758 ) ;
#6891 = ADVANCED_FACE ( 'NONE', ( #21587 ), #17175, .F. ) ;
#6892 = ORIENTED_EDGE ( 'NONE', *, *, #626, .T. ) ;
#6893 = VERTEX_POINT ( 'NONE', #5326 ) ;
#6894 = DIRECTION ( 'NONE',  ( 0.2306359803922019280, 0.9730401042858037863, -1.407521210652539229E-17 ) ) ;
#6895 = SHAPE_REPRESENTATION ( 'Base Frame Plate', ( #18043, #10480, #2866, #18423 ), #11234 ) ;
#6896 = MECHANICAL_CONTEXT ( 'NONE', #22004, 'mechanical' ) ;
#6897 = APPROVAL ( #18866, 'UNKNOWN' ) ;
#6898 = SECURITY_CLASSIFICATION ( '', '', #18135 ) ;
#6899 = DIRECTION ( 'NONE',  ( -0.3034590813640733464, 0.9528444710117558447, -5.155943864260668505E-17 ) ) ;
#6900 = CC_DESIGN_APPROVAL ( #16991, ( #8771 ) ) ;
#6901 = AXIS2_PLACEMENT_3D ( 'NONE', #3545, #8772, #6878 ) ;
#6902 = EDGE_CURVE ( 'NONE', #7324, #20882, #1223, .T. ) ;
#6903 = EDGE_CURVE ( 'NONE', #11858, #12809, #13006, .T. ) ;
#6904 = LOCAL_TIME ( 14, 11, 27.00000000000000000, #5193 ) ;
#6905 = PLANE ( 'NONE',  #18720 ) ;
#6906 = PERSON_AND_ORGANIZATION ( #11966, #8758 ) ;
#6907 = ORIENTED_EDGE ( 'NONE', *, *, #6303, .T. ) ;
#6908 = DIRECTION ( 'NONE',  ( 1.751019220569994795E-16, 2.300154215587015208E-15, 1.000000000000000000 ) ) ;
#6909 = LINE ( 'NONE', #23146, #14302 ) ;
#6910 = VERTEX_POINT ( 'NONE', #20047 ) ;
#6911 = PRODUCT_DEFINITION_FORMATION_WITH_SPECIFIED_SOURCE ( 'ANY', '', #8185, .NOT_KNOWN. ) ;
#6912 = DIRECTION ( 'NONE',  ( 1.164423685541379998E-14, 4.938475812832819565E-14, -1.000000000000000000 ) ) ;
#6913 = DIRECTION ( 'NONE',  ( 0.000000000000000000, -4.196234823359475661E-16, -1.000000000000000000 ) ) ;
#6914 = CARTESIAN_POINT ( 'NONE',  ( 0.4338424296054549933, 18.10873463197630073, -7.340748883243850692E-15 ) ) ;
#6915 = VERTEX_POINT ( 'NONE', #3430 ) ;
#6916 = FACE_OUTER_BOUND ( 'NONE', #19607, .T. ) ;
#6917 = VECTOR ( 'NONE', #1221, 1000.000000000000000 ) ;
#6918 = PERSON_AND_ORGANIZATION ( #11966, #8758 ) ;
#6919 = EDGE_CURVE ( 'NONE', #20612, #3684, #11127, .T. ) ;
#6920 = ORIENTED_EDGE ( 'NONE', *, *, #15857, .T. ) ;
#6921 = AXIS2_PLACEMENT_3D ( 'NONE', #17895, #15765, #3398 ) ;
#6922 = ORIENTED_EDGE ( 'NONE', *, *, #2872, .T. ) ;
#6923 = DIRECTION ( 'NONE',  ( -0.9730401042858036753, 0.2306359803922028995, 5.959266323858677443E-17 ) ) ;
#6924 = VECTOR ( 'NONE', #15369, 1000.000000000000000 ) ;
#6925 = CARTESIAN_POINT ( 'NONE',  ( 33.27705887009660302, -3.036156860536640245, -13.00000000000000000 ) ) ;
#6926 = CARTESIAN_POINT ( 'NONE',  ( 112.5523895830310011, 2.765522746992189695, 3.181688650527689809E-14 ) ) ;
#6927 = PLANE ( 'NONE',  #9562 ) ;
#6928 = PERSON_AND_ORGANIZATION_ROLE ( 'classification_officer' ) ;
#6929 = PLANE ( 'NONE',  #5070 ) ;
#6930 = CC_DESIGN_PERSON_AND_ORGANIZATION_ASSIGNMENT ( #14822, #4490, ( #17927 ) ) ;
#6931 = AXIS2_PLACEMENT_3D ( 'NONE', #8464, #22932, #17610 ) ;
#6932 = APPROVAL ( #20405, 'UNSPECIFIED' ) ;
#6933 = CARTESIAN_POINT ( 'NONE',  ( 41.08211621068439712, 11.24883806106539907, -18.89999999999999858 ) ) ;
#6934 = CIRCLE ( 'NONE', #8829, 0.4000000000000010214 ) ;
#6935 = EDGE_CURVE ( 'NONE', #19931, #15954, #16020, .T. ) ;
#6936 = EDGE_CURVE ( 'NONE', #16935, #677, #16403, .T. ) ;
#6937 = LOCAL_TIME ( 14, 11, 27.00000000000000000, #1147 ) ;
#6938 = APPROVAL ( #2414, 'UNSPECIFIED' ) ;
#6939 = CARTESIAN_POINT ( 'NONE',  ( 0.000000000000000000, 0.000000000000000000, 0.000000000000000000 ) ) ;
#6940 = AXIS2_PLACEMENT_3D ( 'NONE', #4455, #18944, #20833 ) ;
#6941 = ORIENTED_EDGE ( 'NONE', *, *, #1426, .F. ) ;
#6942 = CARTESIAN_POINT ( 'NONE',  ( 112.6956120935900003, 3.369770385951889935, 3.165715546043859906E-14 ) ) ;
#6943 = APPROVAL_ROLE ( '' ) ;
#6944 = CIRCLE ( 'NONE', #2383, 3.500000000000001332 ) ;
#6945 = CARTESIAN_POINT ( 'NONE',  ( -27.50000000434249969, 26.95208919188020147, 8.000000000004540368 ) ) ;
#6946 = CYLINDRICAL_SURFACE ( 'NONE', #14677, 5.000000000000001776 ) ;
#6947 = AXIS2_PLACEMENT_3D ( 'NONE', #8253, #13944, #23069 ) ;
#6948 = DIRECTION ( 'NONE',  ( 0.9730401042858036753, -0.2306359803922028995, 2.740969466505749537E-16 ) ) ;
#6949 = CARTESIAN_POINT ( 'NONE',  ( 43.45766680872420551, 21.27115113520929768, 13.00000000000000000 ) ) ;
#6950 = DIRECTION ( 'NONE',  ( 4.115594265186587621E-36, 2.805478249468460519E-20, 1.000000000000000000 ) ) ;
#6951 = ORIENTED_EDGE ( 'NONE', *, *, #13841, .F. ) ;
#6952 = AXIS2_PLACEMENT_3D ( 'NONE', #16482, #18161, #18281 ) ;
#6953 = DIRECTION ( 'NONE',  ( -0.9730401042858033422, 0.2306359803922031215, -1.141364251305443211E-16 ) ) ;
#6954 = AXIS2_PLACEMENT_3D ( 'NONE', #22182, #22066, #18414 ) ;
#6955 = ADVANCED_FACE ( 'NONE', ( #3315 ), #5453, .F. ) ;
#6956 = PRODUCT_DEFINITION_FORMATION_WITH_SPECIFIED_SOURCE ( 'ANY', '', #15182, .NOT_KNOWN. ) ;
#6957 = ORIENTED_EDGE ( 'NONE', *, *, #33, .T. ) ;
#6958 = LINE ( 'NONE', #13838, #19436 ) ;
#6959 = LINE ( 'NONE', #2907, #18982 ) ;
#6960 = ORIENTED_EDGE ( 'NONE', *, *, #13730, .T. ) ;
#6961 = VECTOR ( 'NONE', #3307, 999.9999999999998863 ) ;
#6962 = AXIS2_PLACEMENT_3D ( 'NONE', #11348, #13341, #22471 ) ;
#6963 = FACE_OUTER_BOUND ( 'NONE', #21644, .T. ) ;
#6964 = EDGE_CURVE ( 'NONE', #17890, #11752, #18045, .T. ) ;
#6965 = ORIENTED_EDGE ( 'NONE', *, *, #11027, .F. ) ;
#6966 = AXIS2_PLACEMENT_3D ( 'NONE', #858, #20811, #11815 ) ;
#6967 = CARTESIAN_POINT ( 'NONE',  ( 35.24824457160688240, 8.315249525024842825, 27.55602540378454535 ) ) ;
#6968 = COORDINATED_UNIVERSAL_TIME_OFFSET ( 0, 0, .AHEAD. ) ;
#6969 = DIRECTION ( 'NONE',  ( -0.9730401042858035643, 0.2306359803922028717, -2.740969466505749044E-16 ) ) ;
#6970 = ADVANCED_FACE ( 'NONE', ( #17930 ), #12705, .F. ) ;
#6971 = EDGE_CURVE ( 'NONE', #3314, #20139, #3769, .T. ) ;
#6972 =( NAMED_UNIT ( * ) PLANE_ANGLE_UNIT ( ) SI_UNIT ( $, .RADIAN. ) );
#6973 = AXIS2_PLACEMENT_3D ( 'NONE', #11355, #22235, #5984 ) ;
#6975 = PLANE ( 'NONE',  #5438 ) ;
#6974 = AXIS2_PLACEMENT_3D ( 'NONE', #22999, #8896, #1500 ) ;
#6976 = CARTESIAN_POINT ( 'NONE',  ( 36.07092311366589854, 11.78608357701213905, -8.759424124907058129 ) ) ;
#6977 = DIRECTION ( 'NONE',  ( 0.000000000000000000, 0.000000000000000000, 1.000000000000000000 ) ) ;
#6978 = SECURITY_CLASSIFICATION ( '', '', #16784 ) ;
#6979 = CARTESIAN_POINT ( 'NONE',  ( -27.39127619791450030, 6.327883175579949615, -2.500000000000000000 ) ) ;
#6980 = AXIS2_PLACEMENT_3D ( 'NONE', #11249, #13361, #19154 ) ;
#6981 = ORIENTED_EDGE ( 'NONE', *, *, #10859, .F. ) ;
#6982 = DIRECTION ( 'NONE',  ( 0.2306359803922080620, 0.9730401042858023430, -1.046328025073550694E-14 ) ) ;
#6983 = CIRCLE ( 'NONE', #18345, 7.000000000000004441 ) ;
#6984 = AXIS2_PLACEMENT_3D ( 'NONE', #17889, #8749, #15871 ) ;
#6985 = CARTESIAN_POINT ( 'NONE',  ( 118.6002496876800052, -6.405594307115129560, 18.89999999999999858 ) ) ;
#6986 = ORIENTED_EDGE ( 'NONE', *, *, #20301, .F. ) ;
#6987 = CARTESIAN_POINT ( 'NONE',  ( 34.07732981382596193, 11.20451025314141624, -8.943038809424274760 ) ) ;
#6988 = FACE_OUTER_BOUND ( 'NONE', #723, .T. ) ;
#6989 = EDGE_LOOP ( 'NONE', ( #3547, #8640, #5466, #19103 ) ) ;
#6990 = PLANE ( 'NONE',  #14501 ) ;
#6991 = ORIENTED_EDGE ( 'NONE', *, *, #10006, .F. ) ;
#6992 = AXIS2_PLACEMENT_3D ( 'NONE', #22557, #4513, #16739 ) ;
#6993 = EDGE_LOOP ( 'NONE', ( #5955, #5556, #6206, #16271 ) ) ;
#6994 = APPROVAL_DATE_TIME ( #16111, #15767 ) ;
#6995 = DIRECTION ( 'NONE',  ( 4.328311834315510110E-15, 1.851928590941880236E-14, -1.000000000000000000 ) ) ;
#6996 = VECTOR ( 'NONE', #14080, 999.9999999999998863 ) ;
#6997 = EDGE_LOOP ( 'NONE', ( #20371, #18432, #12071, #13074, #7451 ) ) ;
#6998 = CARTESIAN_POINT ( 'NONE',  ( 50.90756547144185618, 18.01515514085710734, 2.067000000000035254 ) ) ;
#6999 = EDGE_CURVE ( 'NONE', #12383, #8090, #7469, .T. ) ;
#7000 = DATE_TIME_ROLE ( 'classification_date' ) ;
#7001 = AXIS2_PLACEMENT_3D ( 'NONE', #2128, #2025, #5687 ) ;
#7002 = DATE_AND_TIME ( #21348, #2330 ) ;
#7003 = CARTESIAN_POINT ( 'NONE',  ( -67.73964396923798859, -25.35512988733120565, -1.339745962155620029 ) ) ;
#7004 = FACE_OUTER_BOUND ( 'NONE', #16361, .T. ) ;
#7005 = EDGE_LOOP ( 'NONE', ( #19255, #15398, #6112, #6747 ) ) ;
#7006 = EDGE_CURVE ( 'NONE', #13450, #8538, #3662, .T. ) ;
#7007 = CIRCLE ( 'NONE', #5095, 3.499999999999998668 ) ;
#7008 = ORIENTED_EDGE ( 'NONE', *, *, #21094, .F. ) ;
#7009 = AXIS2_PLACEMENT_3D ( 'NONE', #17802, #16128, #21230 ) ;
#7010 = DIRECTION ( 'NONE',  ( -0.9730401042858024541, 0.2306359803922080898, 5.959266323858942451E-17 ) ) ;
#7011 = DIRECTION ( 'NONE',  ( -0.2306359803922066187, -0.9730401042858026761, 0.000000000000000000 ) ) ;
#7012 = VERTEX_POINT ( 'NONE', #10937 ) ;
#7013 = DIRECTION ( 'NONE',  ( 0.9730401042858024541, -0.2306359803922080898, -5.959266323858942451E-17 ) ) ;
#7014 = CARTESIAN_POINT ( 'NONE',  ( -16.50000000000000000, -20.00000000000000000, -2.500000000000000000 ) ) ;
#7015 = EDGE_LOOP ( 'NONE', ( #5169, #1925, #15429, #6718 ) ) ;
#7016 = ORIENTED_EDGE ( 'NONE', *, *, #12315, .F. ) ;
#7017 = COORDINATED_UNIVERSAL_TIME_OFFSET ( 0, 0, .AHEAD. ) ;
#7018 = VERTEX_POINT ( 'NONE', #12368 ) ;
#7019 = VERTEX_POINT ( 'NONE', #8786 ) ;
#7020 = DIRECTION ( 'NONE',  ( 0.7806762821592939661, -0.6249356306644248127, -7.632783294297949638E-15 ) ) ;
#7021 = DATE_AND_TIME ( #23263, #12991 ) ;
#7022 = DIRECTION ( 'NONE',  ( 0.000000000000000000, 0.000000000000000000, -1.000000000000000000 ) ) ;
#7023 = CALENDAR_DATE ( 2026, 31, 10 ) ;
#7024 = APPLICATION_CONTEXT ( 'configuration controlled 3d designs of mechanical parts and assemblies' ) ;
#7025 = DIRECTION ( 'NONE',  ( -5.163058955534739404E-35, -6.243192354061819367E-17, -1.000000000000000000 ) ) ;
#7026 = EDGE_CURVE ( 'NONE', #14214, #2200, #10585, .T. ) ;
#7027 = EDGE_CURVE ( 'NONE', #12824, #15703, #19083, .T. ) ;
#7028 = APPROVAL_STATUS ( 'not_yet_approved' ) ;
#7029 = PRODUCT_DEFINITION_SHAPE ( 'NONE', 'NONE',  #13725 ) ;
#7030 = ORIENTED_EDGE ( 'NONE', *, *, #22108, .F. ) ;
#7031 = CARTESIAN_POINT ( 'NONE',  ( 96.81657767996070163, -18.09668638014640152, 13.00000000000000000 ) ) ;
#7032 = FACE_OUTER_BOUND ( 'NONE', #11934, .T. ) ;
#7033 = ORIENTED_EDGE ( 'NONE', *, *, #18675, .F. ) ;
#7034 = CARTESIAN_POINT ( 'NONE',  ( -65.82123935389580538, 11.86253283145240012, 5.000000000000000000 ) ) ;
#7035 = AXIS2_PLACEMENT_3D ( 'NONE', #11405, #2119, #443 ) ;
#7036 = CARTESIAN_POINT ( 'NONE',  ( 44.61084671068389440, 26.13635165663700022, 17.99999999999970157 ) ) ;
#7037 = SHAPE_REPRESENTATION ( '1602p_c_04', ( #12739 ), #7801 ) ;
#7038 = LINE ( 'NONE', #21494, #14885 ) ;
#7039 = ORIENTED_EDGE ( 'NONE', *, *, #13073, .F. ) ;
#7040 = ORIENTED_EDGE ( 'NONE', *, *, #5273, .F. ) ;
#7041 = CARTESIAN_POINT ( 'NONE',  ( -12.99532053203719961, 13.48190178978399878, 2.500000000000000000 ) ) ;
#7042 = EDGE_CURVE ( 'NONE', #1184, #2018, #7368, .T. ) ;
#7043 = ADVANCED_FACE ( 'NONE', ( #2352 ), #20518, .F. ) ;
#7044 = PERSON_AND_ORGANIZATION ( #11966, #8758 ) ;
#7045 = ORIENTED_EDGE ( 'NONE', *, *, #10690, .F. ) ;
#7046 = ORIENTED_EDGE ( 'NONE', *, *, #16572, .F. ) ;
#7047 = DIRECTION ( 'NONE',  ( 0.000000000000000000, 0.000000000000000000, 1.000000000000000000 ) ) ;
#7048 = FACE_BOUND ( 'NONE', #6777, .T. ) ;
#7049 = DIRECTION ( 'NONE',  ( -0.9730401042858035643, 0.2306359803922028717, 6.126766849694256332E-17 ) ) ;
#7050 = PERSON_AND_ORGANIZATION ( #11966, #8758 ) ;
#7051 = CARTESIAN_POINT ( 'NONE',  ( 114.9405074087380001, 12.84085624101770051, 2.915350241847199977E-14 ) ) ;
#7052 = LINE ( 'NONE', #14041, #20489 ) ;
#7053 = VECTOR ( 'NONE', #763, 999.9999999999998863 ) ;
#7054 = DIRECTION ( 'NONE',  ( -0.2306359803922076734, -0.9730401042858024541, 1.412237191019896754E-17 ) ) ;
#7055 = EDGE_CURVE ( 'NONE', #16863, #22020, #20969, .T. ) ;
#7056 = COORDINATED_UNIVERSAL_TIME_OFFSET ( 0, 0, .AHEAD. ) ;
#7057 = CARTESIAN_POINT ( 'NONE',  ( 3.747449283612720006, 22.11622885388230131, 4.500000000000000000 ) ) ;
#7058 = DIRECTION ( 'NONE',  ( -3.210834492194360164E-17, 2.441916418604790135E-15, 1.000000000000000000 ) ) ;
#7059 = CC_DESIGN_DATE_AND_TIME_ASSIGNMENT ( #19190, #15616, ( #5063 ) ) ;
#7060 = DIRECTION ( 'NONE',  ( -0.9997651245102161521, -0.02167246670483386276, 0.000000000000000000 ) ) ;
#7061 = DIRECTION ( 'NONE',  ( 0.9730401042858024541, -0.2306359803922080898, -5.959266323858942451E-17 ) ) ;
#7062 = CC_DESIGN_DATE_AND_TIME_ASSIGNMENT ( #9765, #2386, ( #15459 ) ) ;
#7063 = DIRECTION ( 'NONE',  ( 0.9579954394086668268, 0.2867834340965239592, -1.485305508172449974E-15 ) ) ;
#7064 = VERTEX_POINT ( 'NONE', #16590 ) ;
#7065 = DIRECTION ( 'NONE',  ( -1.000000000000000000, 0.000000000000000000, 0.000000000000000000 ) ) ;
#7066 = EDGE_CURVE ( 'NONE', #15508, #8933, #14821, .T. ) ;
#7067 = EDGE_CURVE ( 'NONE', #22148, #13627, #1241, .T. ) ;
#7068 = AXIS2_PLACEMENT_3D ( 'NONE', #5139, #21511, #23298 ) ;
#7069 = ADVANCED_FACE ( 'NONE', ( #15169 ), #678, .T. ) ;
#7070 = ORIENTED_EDGE ( 'NONE', *, *, #22705, .T. ) ;
#7071 = FACE_OUTER_BOUND ( 'NONE', #19559, .T. ) ;
#7072 = FACE_OUTER_BOUND ( 'NONE', #1730, .T. ) ;
#7073 = EDGE_CURVE ( 'NONE', #2422, #563, #1993, .T. ) ;
#7074 = ORIENTED_EDGE ( 'NONE', *, *, #19989, .T. ) ;
#7075 = CARTESIAN_POINT ( 'NONE',  ( 6.500000000000000000, -17.30000000000000071, 5.000000000000000000 ) ) ;
#7076 = CIRCLE ( 'NONE', #4768, 15.25000000000000000 ) ;
#7077 = ORIENTED_EDGE ( 'NONE', *, *, #782, .T. ) ;
#7078 = FACE_OUTER_BOUND ( 'NONE', #5356, .T. ) ;
#7079 = APPROVAL_ROLE ( '' ) ;
#7080 = CARTESIAN_POINT ( 'NONE',  ( -26.68810977484059777, -6.639828994528159889, 9.265539023039960360E-14 ) ) ;
#7081 = FACE_OUTER_BOUND ( 'NONE', #10173, .T. ) ;
#7082 = DIRECTION ( 'NONE',  ( 0.2306359803922017615, 0.9730401042858037863, -3.356987858687580135E-15 ) ) ;
#7083 = EDGE_CURVE ( 'NONE', #18750, #15392, #6168, .T. ) ;
#7084 = CIRCLE ( 'NONE', #13900, 6.000000000000000000 ) ;
#7085 = VECTOR ( 'NONE', #6948, 999.9999999999998863 ) ;
#7086 = CARTESIAN_POINT ( 'NONE',  ( 39.69419854219519550, 9.774809681453278998, 23.00000000000000000 ) ) ;
#7087 = LINE ( 'NONE', #5632, #19625 ) ;
#7088 = CARTESIAN_POINT ( 'NONE',  ( -67.10928800542700401, -21.60172791560102112, -6.068947416084667781E-15 ) ) ;
#7089 = CARTESIAN_POINT ( 'NONE',  ( -20.00000001665348037, -17.50000000000000000, 8.000000000004535039 ) ) ;
#7090 = ORIENTED_EDGE ( 'NONE', *, *, #7454, .T. ) ;
#7091 = DIRECTION ( 'NONE',  ( 0.000000000000000000, 0.000000000000000000, 1.000000000000000000 ) ) ;
#7092 = FACE_OUTER_BOUND ( 'NONE', #21578, .T. ) ;
#7093 = EDGE_CURVE ( 'NONE', #17221, #1017, #19452, .T. ) ;
#7095 = VERTEX_POINT ( 'NONE', #6034 ) ;
#7094 = ADVANCED_FACE ( 'NONE', ( #16845, #11399, #18638, #317, #20177, #22409 ), #7820, .F. ) ;
#7096 = DIRECTION ( 'NONE',  ( 0.000000000000000000, 1.000000000000000000, -9.605990953944227443E-124 ) ) ;
#7097 = EDGE_LOOP ( 'NONE', ( #19792, #1868, #2403 ) ) ;
#7098 = ORIENTED_EDGE ( 'NONE', *, *, #6964, .F. ) ;
#7099 = SECURITY_CLASSIFICATION_LEVEL ( 'unclassified' ) ;
#7100 = CARTESIAN_POINT ( 'NONE',  ( 41.08211621068439712, 11.24883806106539907, -19.59999999999999787 ) ) ;
#7101 = ORIENTED_EDGE ( 'NONE', *, *, #5727, .T. ) ;
#7102 = CIRCLE ( 'NONE', #8619, 15.25000000000000000 ) ;
#7103 = DIRECTION ( 'NONE',  ( 0.2306359803922031215, 0.9730401042858033422, -1.407521210652540462E-17 ) ) ;
#7104 = CALENDAR_DATE ( 2026, 31, 10 ) ;
#7105 = ITEM_DEFINED_TRANSFORMATION ( 'NONE', 'NONE', #7068,  #12739 ) ;
#7106 = DIRECTION ( 'NONE',  ( 0.2306359803922085339, 0.9730401042858022320, 0.000000000000000000 ) ) ;
#7107 = PERSON ( 'NAUO-PER3', 'UNSPECIFIED', 'UNSPECIFIED', ('UNSPECIFIED'), ('UNSPECIFIED'), ('UNSPECIFIED') ) ;
#7108 = EDGE_CURVE ( 'NONE', #10921, #1846, #15271, .T. ) ;
#7109 = VECTOR ( 'NONE', #16523, 1000.000000000000000 ) ;
#7110 = LINE ( 'NONE', #19800, #14553 ) ;
#7111 = VERTEX_POINT ( 'NONE', #4253 ) ;
#7112 = LINE ( 'NONE', #1740, #13232 ) ;
#7113 = AXIS2_PLACEMENT_3D ( 'NONE', #7766, #10998, #11473 ) ;
#7114 = AXIS2_PLACEMENT_3D ( 'NONE', #5572, #453, #18418 ) ;
#7115 = ORIENTED_EDGE ( 'NONE', *, *, #19571, .T. ) ;
#7116 = DIRECTION ( 'NONE',  ( -2.270069654138870255E-15, -1.000000000000000000, -7.035747901516317327E-77 ) ) ;
#7117 = CARTESIAN_POINT ( 'NONE',  ( 2.500000000000000000, -31.09999999999999787, -21.50000000000000000 ) ) ;
#7118 = CARTESIAN_POINT ( 'NONE',  ( -8.080225385240000335, -15.72171916155420313, -5.000000000000000000 ) ) ;
#7119 = VERTEX_POINT ( 'NONE', #7582 ) ;
#7120 = EDGE_CURVE ( 'NONE', #6299, #19075, #12174, .T. ) ;
#7121 = EDGE_CURVE ( 'NONE', #17345, #6764, #11293, .T. ) ;
#7122 = FACE_OUTER_BOUND ( 'NONE', #3984, .T. ) ;
#7123 = LINE ( 'NONE', #8664, #16425 ) ;
#7124 = AXIS2_PLACEMENT_3D ( 'NONE', #512, #5866, #20464 ) ;
#7125 = EDGE_LOOP ( 'NONE', ( #19003, #18968, #22936, #18839 ) ) ;
#7126 = VERTEX_POINT ( 'NONE', #17297 ) ;
#7127 = PERSON_AND_ORGANIZATION ( #11966, #8758 ) ;
#7128 = ORIENTED_EDGE ( 'NONE', *, *, #8356, .T. ) ;
#7129 = ORIENTED_EDGE ( 'NONE', *, *, #10588, .T. ) ;
#7130 = VECTOR ( 'NONE', #3219, 1000.000000000000000 ) ;
#7131 = APPROVAL_STATUS ( 'not_yet_approved' ) ;
#7132 = AXIS2_PLACEMENT_3D ( 'NONE', #10074, #3508, #17881 ) ;
#7133 = AXIS2_PLACEMENT_3D ( 'NONE', #17018, #4332, #11600 ) ;
#7134 = DIRECTION ( 'NONE',  ( 0.5021071549687922131, -0.8648054144888001060, 0.000000000000000000 ) ) ;
#7135 = CONTEXT_DEPENDENT_SHAPE_REPRESENTATION ( #4325, #20494 ) ;
#7136 = CIRCLE ( 'NONE', #6375, 2.499999999999998668 ) ;
#7137 = DIRECTION ( 'NONE',  ( 0.000000000000000000, 0.000000000000000000, 1.000000000000000000 ) ) ;
#7138 = AXIS2_PLACEMENT_3D ( 'NONE', #17431, #1145, #4837 ) ;
#7139 = PRODUCT_DEFINITION ( 'UNKNOWN', '', #11812, #14873 ) ;
#7140 = APPROVAL_ROLE ( '' ) ;
#7141 = VERTEX_POINT ( 'NONE', #10301 ) ;
#7142 = AXIS2_PLACEMENT_3D ( 'NONE', #18958, #6482, #15858 ) ;
#7143 = DIRECTION ( 'NONE',  ( 1.000000000000000000, 6.123237831918419028E-17, 0.000000000000000000 ) ) ;
#7144 = CARTESIAN_POINT ( 'NONE',  ( 33.90884364377009774, 10.17428291754630010, 27.68999999999999773 ) ) ;
#7145 = ORIENTED_EDGE ( 'NONE', *, *, #22822, .T. ) ;
#7146 = DIRECTION ( 'NONE',  ( 9.248890187689720549E-11, -1.000000000000000000, 2.220446048198180498E-15 ) ) ;
#7148 = CIRCLE ( 'NONE', #20413, 2.499999999999998668 ) ;
#7147 = CARTESIAN_POINT ( 'NONE',  ( 35.01760859121468883, 7.342209420739032488, 26.30000000000001137 ) ) ;
#7149 = CARTESIAN_POINT ( 'NONE',  ( 28.14554285793940025, -3.006546890859489896, 15.00000000000000000 ) ) ;
#7150 = ORIENTED_EDGE ( 'NONE', *, *, #20881, .F. ) ;
#7151 = ORIENTED_EDGE ( 'NONE', *, *, #12692, .T. ) ;
#7152 = LINE ( 'NONE', #5476, #9111 ) ;
#7153 = ORIENTED_EDGE ( 'NONE', *, *, #9879, .F. ) ;
#7154 = CALENDAR_DATE ( 2026, 31, 10 ) ;
#7155 = ORIENTED_EDGE ( 'NONE', *, *, #22538, .T. ) ;
#7156 = ORIENTED_EDGE ( 'NONE', *, *, #6641, .T. ) ;
#7157 = CARTESIAN_POINT ( 'NONE',  ( 35.84667945578014780, -10.83917230622373928, -16.00000000000000000 ) ) ;
#7158 = FACE_OUTER_BOUND ( 'NONE', #19583, .T. ) ;
#7159 = DIRECTION ( 'NONE',  ( -1.000000000000000000, 0.000000000000000000, 0.000000000000000000 ) ) ;
#7160 = COORDINATED_UNIVERSAL_TIME_OFFSET ( 0, 0, .AHEAD. ) ;
#7161 = CARTESIAN_POINT ( 'NONE',  ( 113.2033677465029911, -29.17473274740279976, -13.00000000000000000 ) ) ;
#7162 = ADVANCED_FACE ( 'NONE', ( #12088 ), #6480, .F. ) ;
#7163 = LINE ( 'NONE', #14389, #4951 ) ;
#7164 = CIRCLE ( 'NONE', #15880, 4.999999999999998224 ) ;
#7165 = DIRECTION ( 'NONE',  ( 0.000000000000000000, 0.000000000000000000, 1.000000000000000000 ) ) ;
#7166 = ADVANCED_FACE ( 'NONE', ( #17529 ), #13851, .T. ) ;
#7167 = CARTESIAN_POINT ( 'NONE',  ( 35.01760859121470304, 7.342209420738848635, -10.99076000000048836 ) ) ;
#7168 = CALENDAR_DATE ( 2026, 31, 10 ) ;
#7169 = SHAPE_REPRESENTATION ( '1602p_c_14', ( #12739 ), #210 ) ;
#7170 = LINE ( 'NONE', #12636, #4154 ) ;
#7171 = DIRECTION ( 'NONE',  ( -0.9997648975362221080, -0.02168293463503390486, 0.000000000000000000 ) ) ;
#7172 = LINE ( 'NONE', #21518, #15801 ) ;
#7173 = CARTESIAN_POINT ( 'NONE',  ( -20.00000000000190070, -20.00000000000000000, -8.499999999995459632 ) ) ;
#7174 = DIRECTION ( 'NONE',  ( 0.000000000000000000, 0.000000000000000000, 1.000000000000000000 ) ) ;
#7175 = EDGE_LOOP ( 'NONE', ( #17826, #18204, #1075, #6855 ) ) ;
#7176 = CARTESIAN_POINT ( 'NONE',  ( 35.93758199568961942, 11.81768891304677815, 8.759424124907043918 ) ) ;
#7177 = ORIENTED_EDGE ( 'NONE', *, *, #8477, .T. ) ;
#7178 = CARTESIAN_POINT ( 'NONE',  ( -20.00000000397270128, 22.95208919257159863, 5.000000000004460432 ) ) ;
#7179 = DIRECTION ( 'NONE',  ( -1.000000000000000000, 2.270069654138870255E-15, -3.099353312215988811E-62 ) ) ;
#7180 = VERTEX_POINT ( 'NONE', #14074 ) ;
#7181 = CARTESIAN_POINT ( 'NONE',  ( 35.01760859121468172, 7.342209420738772252, -26.30000000000049099 ) ) ;
#7182 = EDGE_CURVE ( 'NONE', #23367, #16446, #8074, .T. ) ;
#7183 = VERTEX_POINT ( 'NONE', #11973 ) ;
#7184 = DIRECTION ( 'NONE',  ( 0.9730401042858035643, -0.2306359803922028717, -5.959266323858677443E-17 ) ) ;
#7185 = COORDINATED_UNIVERSAL_TIME_OFFSET ( 0, 0, .AHEAD. ) ;
#7186 = AXIS2_PLACEMENT_3D ( 'NONE', #19529, #8851, #17403 ) ;
#7187 = LINE ( 'NONE', #10886, #15450 ) ;
#7188 = CC_DESIGN_PERSON_AND_ORGANIZATION_ASSIGNMENT ( #16233, #294, ( #22797 ) ) ;
#7189 = DIRECTION ( 'NONE',  ( 0.8846153846154060085, -0.4663213712685030377, 0.000000000000000000 ) ) ;
#7190 = EDGE_CURVE ( 'NONE', #23222, #11662, #8733, .T. ) ;
#7191 = ADVANCED_FACE ( 'NONE', ( #19194 ), #15622, .T. ) ;
#7192 = CARTESIAN_POINT ( 'NONE',  ( 113.2956221386590130, -28.78551670568849730, 2.700000000000000178 ) ) ;
#7193 = DIRECTION ( 'NONE',  ( 1.000000000000000000, 0.000000000000000000, 0.000000000000000000 ) ) ;
#7194 = CARTESIAN_POINT ( 'NONE',  ( 120.8143550994449953, 2.935590694028619829, -20.00000000000000000 ) ) ;
#7195 =( REPRESENTATION_RELATIONSHIP ('NONE','NONE', #18771, #8415 ) REPRESENTATION_RELATIONSHIP_WITH_TRANSFORMATION ( #15356 )SHAPE_REPRESENTATION_RELATIONSHIP( ) );
#7196 = FACE_OUTER_BOUND ( 'NONE', #4395, .T. ) ;
#7197 = DIRECTION ( 'NONE',  ( -0.9730401042858035643, 0.2306359803922028717, 5.958148513035547083E-17 ) ) ;
#7198 = DIRECTION ( 'NONE',  ( -1.000000000000000000, 0.000000000000000000, 0.000000000000000000 ) ) ;
#7199 = ORIENTED_EDGE ( 'NONE', *, *, #595, .T. ) ;
#7200 = LOCAL_TIME ( 14, 11, 27.00000000000000000, #9369 ) ;
#7201 = DIRECTION ( 'NONE',  ( 0.000000000000000000, 1.156482317317871478E-16, 1.000000000000000000 ) ) ;
#7202 = CIRCLE ( 'NONE', #5655, 4.999999999999997335 ) ;
#7203 = DIRECTION ( 'NONE',  ( -1.000000000000000000, 0.000000000000000000, 7.691776389375310104E-16 ) ) ;
#7204 = VERTEX_POINT ( 'NONE', #1469 ) ;
#7205 = CARTESIAN_POINT ( 'NONE',  ( 114.9904400984929254, 13.05151942359561801, -2.500000000000011990 ) ) ;
#7206 = DIRECTION ( 'NONE',  ( -0.1153179901961009640, -0.4865200521429018377, 0.8660254037844385966 ) ) ;
#7207 = ORIENTED_EDGE ( 'NONE', *, *, #5915, .F. ) ;
#7208 = PERSON_AND_ORGANIZATION ( #11966, #8758 ) ;
#7209 = FACE_OUTER_BOUND ( 'NONE', #18973, .T. ) ;
#7210 = EDGE_CURVE ( 'NONE', #4832, #851, #10069, .T. ) ;
#7211 = EDGE_LOOP ( 'NONE', ( #1806, #5382, #10169, #10983 ) ) ;
#7212 = DIRECTION ( 'NONE',  ( 1.138590270679730064E-14, 2.220446049251240387E-15, 1.000000000000000000 ) ) ;
#7213 = PERSON_AND_ORGANIZATION ( #11966, #8758 ) ;
#7214 = CC_DESIGN_PERSON_AND_ORGANIZATION_ASSIGNMENT ( #11184, #21937, ( #1599 ) ) ;
#7215 = PRODUCT ( '1602p_c_21', '1602p_c_21', '', ( #11990 ) ) ;
#7216 = CC_DESIGN_PERSON_AND_ORGANIZATION_ASSIGNMENT ( #15550, #3204, ( #6875 ) ) ;
#7217 = CONTEXT_DEPENDENT_SHAPE_REPRESENTATION ( #16131, #3779 ) ;
#7218 = AXIS2_PLACEMENT_3D ( 'NONE', #19189, #19302, #3023 ) ;
#7219 = DIRECTION ( 'NONE',  ( 0.8648054144888007722, 0.5021071549687909918, -4.823236788540877710E-124 ) ) ;
#7220 = CIRCLE ( 'NONE', #4546, 2.999765877365279998 ) ;
#7221 = EDGE_CURVE ( 'NONE', #7012, #8111, #22862, .T. ) ;
#7222 = ADVANCED_FACE ( 'NONE', ( #22864 ), #1242, .F. ) ;
#7223 = CARTESIAN_POINT ( 'NONE',  ( 35.01760859121468883, 7.342209420738806891, -19.99999999999998579 ) ) ;
#7224 = EDGE_LOOP ( 'NONE', ( #14371, #17481, #12620, #17671, #14966 ) ) ;
#7225 = DIRECTION ( 'NONE',  ( -0.005225493778937319485, 0.9999863470141810984, -2.442038948240150648E-15 ) ) ;
#7226 = EDGE_LOOP ( 'NONE', ( #9275, #11663, #916, #2350 ) ) ;
#7227 = DIRECTION ( 'NONE',  ( -0.5021071549687922131, 0.8648054144888001060, 0.000000000000000000 ) ) ;
#7228 = CARTESIAN_POINT ( 'NONE',  ( 43.87899317387989839, 21.17128575569940097, -13.00000000000000000 ) ) ;
#7229 = CARTESIAN_POINT ( 'NONE',  ( -69.83648240813081998, -6.865755409778300233, -5.500000000000079048 ) ) ;
#7230 = ORIENTED_EDGE ( 'NONE', *, *, #17042, .F. ) ;
#7231 = PRODUCT_DEFINITION_FORMATION_WITH_SPECIFIED_SOURCE ( 'ANY', '', #15912, .NOT_KNOWN. ) ;
#7232 = DIRECTION ( 'NONE',  ( -0.2306359803922053142, -0.9730401042858028982, 0.000000000000000000 ) ) ;
#7233 = CARTESIAN_POINT ( 'NONE',  ( 52.49909637502329929, -7.592283011512620305, -15.25462000000040064 ) ) ;
#7234 = AXIS2_PLACEMENT_3D ( 'NONE', #23209, #19657, #1594 ) ;
#7235 = VERTEX_POINT ( 'NONE', #12202 ) ;
#7236 = PERSON_AND_ORGANIZATION ( #11966, #8758 ) ;
#7237 = EDGE_CURVE ( 'NONE', #22814, #10370, #15665, .T. ) ;
#7238 = ORIENTED_EDGE ( 'NONE', *, *, #6199, .T. ) ;
#7239 = VERTEX_POINT ( 'NONE', #2919 ) ;
#7240 = CARTESIAN_POINT ( 'NONE',  ( -12.59661859122890171, -1.225550774622820027, 8.000000000004430234 ) ) ;
#7241 = CALENDAR_DATE ( 2026, 31, 10 ) ;
#7242 = CIRCLE ( 'NONE', #5328, 2.369999999999999218 ) ;
#7243 = EDGE_CURVE ( 'NONE', #19931, #3332, #14159, .T. ) ;
#7244 = DIRECTION ( 'NONE',  ( 2.982858504577314686E-17, -2.441916418604790135E-15, -1.000000000000000000 ) ) ;
#7245 = DATE_AND_TIME ( #7586, #12872 ) ;
#7246 = DIRECTION ( 'NONE',  ( -4.028143194477080210E-16, -2.054129435991050111E-15, -1.000000000000000000 ) ) ;
#7247 = ADVANCED_FACE ( 'NONE', ( #10426 ), #11919, .F. ) ;
#7248 = LOCAL_TIME ( 14, 11, 27.00000000000000000, #20202 ) ;
#7249 = EDGE_CURVE ( 'NONE', #7455, #9721, #17654, .T. ) ;
#7250 = LOCAL_TIME ( 14, 11, 27.00000000000000000, #9915 ) ;
#7251 = DIRECTION ( 'NONE',  ( -0.2306359803922053697, -0.9730401042858028982, 0.000000000000000000 ) ) ;
#7252 = VECTOR ( 'NONE', #8046, 1000.000000000000000 ) ;
#7253 = COORDINATED_UNIVERSAL_TIME_OFFSET ( 0, 0, .AHEAD. ) ;
#7254 = LOCAL_TIME ( 14, 11, 27.00000000000000000, #11747 ) ;
#7255 = ORIENTED_EDGE ( 'NONE', *, *, #1980, .F. ) ;
#7256 = CARTESIAN_POINT ( 'NONE',  ( 58.49563186522070168, 17.70675969991879839, -13.00000000000049916 ) ) ;
#7257 = AXIS2_PLACEMENT_3D ( 'NONE', #9569, #22596, #15367 ) ;
#7258 = ORIENTED_EDGE ( 'NONE', *, *, #19877, .F. ) ;
#7259 = DIRECTION ( 'NONE',  ( 0.000000000000000000, 0.000000000000000000, 1.000000000000000000 ) ) ;
#7260 = DIRECTION ( 'NONE',  ( 0.005235963827102643048, -0.9999862922474495042, -7.724582913192744961E-15 ) ) ;
#7261 = CARTESIAN_POINT ( 'NONE',  ( 32.96699026062353255, 10.39752682851250576, 26.49999999999999645 ) ) ;
#7262 = EDGE_LOOP ( 'NONE', ( #15460, #12068, #16306, #4376 ) ) ;
#7263 = ORIENTED_EDGE ( 'NONE', *, *, #3233, .T. ) ;
#7264 = DIRECTION ( 'NONE',  ( 0.7806762821593211665, -0.6249356306643909509, -7.632783294297951215E-15 ) ) ;
#7265 = EDGE_LOOP ( 'NONE', ( #22520, #5282, #12354, #6750, #4245 ) ) ;
#7266 = SECURITY_CLASSIFICATION_LEVEL ( 'unclassified' ) ;
#7267 = LOCAL_TIME ( 14, 11, 27.00000000000000000, #10227 ) ;
#7268 = EDGE_LOOP ( 'NONE', ( #309, #3832, #5760, #23366 ) ) ;
#7269 = EDGE_LOOP ( 'NONE', ( #19096, #3096, #22523, #12865 ) ) ;
#7270 = FACE_OUTER_BOUND ( 'NONE', #14855, .T. ) ;
#7271 = APPROVAL_PERSON_ORGANIZATION ( #15336, #17427, #21139 ) ;
#7272 = DIRECTION ( 'NONE',  ( 5.798605125234323991E-17, -1.374421231021384554E-17, 1.000000000000000000 ) ) ;
#7273 = PERSON_AND_ORGANIZATION ( #11966, #8758 ) ;
#7274 = CIRCLE ( 'NONE', #6901, 3.499999999999998668 ) ;
#7275 = CC_DESIGN_DATE_AND_TIME_ASSIGNMENT ( #18445, #2151, ( #4599 ) ) ;
#7276 = CARTESIAN_POINT ( 'NONE',  ( 0.03403376487640590031, -6.499910899608420500, -8.889944397045749129E-14 ) ) ;
#7277 = DIRECTION ( 'NONE',  ( -0.9730401042858022320, 0.2306359803922080343, 5.959266323858951079E-17 ) ) ;
#7278 = LOCAL_TIME ( 14, 11, 27.00000000000000000, #15653 ) ;
#7279 = ORIENTED_EDGE ( 'NONE', *, *, #6628, .F. ) ;
#7280 = DIRECTION ( 'NONE',  ( 0.8648054144888008832, 0.5021071549687909918, 0.000000000000000000 ) ) ;
#7281 = DATE_AND_TIME ( #10975, #9160 ) ;
#7282 = LOCAL_TIME ( 14, 11, 27.00000000000000000, #7699 ) ;
#7283 = DIRECTION ( 'NONE',  ( 0.9730401042858024541, -0.2306359803922080898, -5.959266323858912869E-17 ) ) ;
#7284 = AXIS2_PLACEMENT_3D ( 'NONE', #12913, #9925, #17155 ) ;
#7285 = LINE ( 'NONE', #21517, #250 ) ;
#7286 = CARTESIAN_POINT ( 'NONE',  ( -20.00000000000000000, -17.50000000000000000, -5.499999999995474731 ) ) ;
#7287 = ADVANCED_FACE ( 'NONE', ( #15503 ), #1356, .T. ) ;
#7288 = CARTESIAN_POINT ( 'NONE',  ( 113.2956221386590130, -28.78551670568849730, 3.100000000000000089 ) ) ;
#7289 = DIRECTION ( 'NONE',  ( 5.964507377817269296E-17, 4.861311874385510251E-15, 1.000000000000000000 ) ) ;
#7290 = ORIENTED_EDGE ( 'NONE', *, *, #8922, .T. ) ;
#7291 = CC_DESIGN_SECURITY_CLASSIFICATION ( #13355, ( #23498 ) ) ;
#7292 = CARTESIAN_POINT ( 'NONE',  ( 33.83992520232241930, 10.87628626253941277, 8.976109897029353135 ) ) ;
#7293 = UNCERTAINTY_MEASURE_WITH_UNIT (LENGTH_MEASURE( 1.000000000000000082E-05 ), #20115, 'distance_accuracy_value', 'NONE');
#7294 = ORIENTED_EDGE ( 'NONE', *, *, #8856, .F. ) ;
#7295 = DIRECTION ( 'NONE',  ( 3.210834492181045054E-17, -2.441916418604790135E-15, -1.000000000000000000 ) ) ;
#7296 = LINE ( 'NONE', #16533, #17815 ) ;
#7297 = ORIENTED_EDGE ( 'NONE', *, *, #19898, .F. ) ;
#7298 = CARTESIAN_POINT ( 'NONE',  ( 28.89837840081079889, -1.998294948772289858, -13.00000000000039968 ) ) ;
#7299 = VERTEX_POINT ( 'NONE', #8621 ) ;
#7300 = LOCAL_TIME ( 14, 11, 27.00000000000000000, #2038 ) ;
#7301 = DIRECTION ( 'NONE',  ( -6.662111140531837817E-09, 1.000000000000000000, -2.081668171172169697E-15 ) ) ;
#7302 = COORDINATED_UNIVERSAL_TIME_OFFSET ( 0, 0, .AHEAD. ) ;
#7303 = VECTOR ( 'NONE', #10027, 1000.000000000000000 ) ;
#7304 = DIRECTION ( 'NONE',  ( 0.005235963827108302583, -0.9999862922474493931, -5.936218956694023463E-19 ) ) ;
#7305 = VECTOR ( 'NONE', #12218, 1000.000000000000000 ) ;
#7306 = AXIS2_PLACEMENT_3D ( 'NONE', #9092, #16324, #16666 ) ;
#7307 =( BOUNDED_CURVE ( )  B_SPLINE_CURVE ( 2, ( #2556, #11836, #10060 ),
 .UNSPECIFIED., .F., .F. ) 
 B_SPLINE_CURVE_WITH_KNOTS ( ( 3, 3 ),
 ( 0.1168436138077930952, 0.2336872276155859962 ),
 .UNSPECIFIED. ) 
 CURVE ( )  GEOMETRIC_REPRESENTATION_ITEM ( )  RATIONAL_B_SPLINE_CURVE ( ( 1.077350269189629950, 1.077350269189629728, 1.000000000000000000 ) ) 
 REPRESENTATION_ITEM ( '' )  );
#7308 = LOCAL_TIME ( 14, 11, 27.00000000000000000, #20041 ) ;
#7309 = FACE_OUTER_BOUND ( 'NONE', #7499, .T. ) ;
#7310 = CARTESIAN_POINT ( 'NONE',  ( -28.45655959278310121, -6.649088660734180145, 0.7325259402522749097 ) ) ;
#7311 = PERSON_AND_ORGANIZATION_ROLE ( 'creator' ) ;
#7312 = CARTESIAN_POINT ( 'NONE',  ( 37.48968750243700043, 22.68571848161319693, -11.84529946162124858 ) ) ;
#7313 = VECTOR ( 'NONE', #16366, 1000.000000000000114 ) ;
#7314 = CARTESIAN_POINT ( 'NONE',  ( 34.24686308852899685, 12.59635270528730011, -5.000000000000000000 ) ) ;
#7315 = DIRECTION ( 'NONE',  ( 0.000000000000000000, 0.000000000000000000, 1.000000000000000000 ) ) ;
#7316 = EDGE_CURVE ( 'NONE', #13648, #554, #4581, .T. ) ;
#7317 = DESIGN_CONTEXT ( 'detailed design', #4758, 'design' ) ;
#7318 = SECURITY_CLASSIFICATION ( '', '', #1382 ) ;
#7319 = DIRECTION ( 'NONE',  ( -2.269700743865584947E-13, -2.220446049247695246E-15, -1.000000000000000000 ) ) ;
#7320 = DIRECTION ( 'NONE',  ( 0.4188360644630711449, 0.9080618652410672453, -2.204917890671980836E-15 ) ) ;
#7321 = AXIS2_PLACEMENT_3D ( 'NONE', #11456, #18807, #4313 ) ;
#7322 = DIRECTION ( 'NONE',  ( 0.9822591002358885826, -0.1875288244611549582, 4.336808689942019215E-16 ) ) ;
#7323 = CIRCLE ( 'NONE', #20591, 2.499999999999998668 ) ;
#7324 = VERTEX_POINT ( 'NONE', #11851 ) ;
#7325 = AXIS2_PLACEMENT_3D ( 'NONE', #21798, #7668, #405 ) ;
#7326 = ORIENTED_EDGE ( 'NONE', *, *, #16363, .F. ) ;
#7327 = CARTESIAN_POINT ( 'NONE',  ( 37.01481097301078194, 22.79827665208033594, 11.00000000000000178 ) ) ;
#7328 = DIRECTION ( 'NONE',  ( 0.2306359803922089224, 0.9730401042858022320, -4.744007713284281141E-15 ) ) ;
#7329 = EDGE_LOOP ( 'NONE', ( #18779, #6951, #6162 ) ) ;
#7330 = EDGE_CURVE ( 'NONE', #2287, #16704, #19085, .T. ) ;
#7331 = EDGE_CURVE ( 'NONE', #12726, #851, #7336, .T. ) ;
#7332 = CALENDAR_DATE ( 2026, 31, 10 ) ;
#7333 = CARTESIAN_POINT ( 'NONE',  ( 4.267766952966368876, -28.60000000000000142, -20.76776695296636888 ) ) ;
#7334 = VERTEX_POINT ( 'NONE', #3728 ) ;
#7335 = DIRECTION ( 'NONE',  ( 0.1187863113461967018, 0.5011527021216418687, 0.8571673007021100021 ) ) ;
#7336 = CIRCLE ( 'NONE', #2411, 7.999999999999998224 ) ;
#7337 = PERSON_AND_ORGANIZATION_ROLE ( 'design_supplier' ) ;
#7338 = CIRCLE ( 'NONE', #5803, 2.458500000000000352 ) ;
#7339 = LOCAL_TIME ( 14, 11, 27.00000000000000000, #15266 ) ;
#7340 = APPROVAL_DATE_TIME ( #10917, #4416 ) ;
#7341 = FACE_OUTER_BOUND ( 'NONE', #5640, .T. ) ;
#7342 = AXIS2_PLACEMENT_3D ( 'NONE', #13303, #20425, #14962 ) ;
#7343 = CIRCLE ( 'NONE', #110, 2.500000000000000444 ) ;
#7344 = CARTESIAN_POINT ( 'NONE',  ( -20.22823963489775068, 17.95730124203003442, 5.500000000004473755 ) ) ;
#7345 = EDGE_LOOP ( 'NONE', ( #6636, #23158 ) ) ;
#7346 = LINE ( 'NONE', #14579, #12111 ) ;
#7347 = EDGE_CURVE ( 'NONE', #13560, #9664, #21357, .T. ) ;
#7348 = ORIENTED_EDGE ( 'NONE', *, *, #18238, .T. ) ;
#7349 = VECTOR ( 'NONE', #21400, 1000.000000000000227 ) ;
#7350 = CARTESIAN_POINT ( 'NONE',  ( 117.1933702072879981, -12.34113894325849969, 19.59999999999999787 ) ) ;
#7351 = DIRECTION ( 'NONE',  ( 0.000000000000000000, -2.738683416504465444E-14, -1.000000000000000000 ) ) ;
#7352 = DIRECTION ( 'NONE',  ( -1.000000000000000000, 0.000000000000000000, 0.000000000000000000 ) ) ;
#7353 = ORIENTED_EDGE ( 'NONE', *, *, #16219, .T. ) ;
#7354 = CC_DESIGN_PERSON_AND_ORGANIZATION_ASSIGNMENT ( #1967, #5191, ( #10554 ) ) ;
#7355 = ORGANIZATION ( 'NAUO-ORG1', 'UNSPECIFIED', 'UNSPECIFIED' ) ;
#7356 = DATE_AND_TIME ( #13726, #18290 ) ;
#7357 = APPROVAL ( #3521, 'UNSPECIFIED' ) ;
#7358 = DIRECTION ( 'NONE',  ( -0.005235963827117092427, 0.9999862922474493931, 2.636227439667000721E-16 ) ) ;
#7359 = CIRCLE ( 'NONE', #6980, 3.499999999999999556 ) ;
#7360 = ORIENTED_EDGE ( 'NONE', *, *, #3915, .F. ) ;
#7361 = ADVANCED_FACE ( 'NONE', ( #7081 ), #157, .T. ) ;
#7362 = EDGE_CURVE ( 'NONE', #22740, #5418, #10774, .T. ) ;
#7363 = APPROVAL_ROLE ( '' ) ;
#7364 = VERTEX_POINT ( 'NONE', #21537 ) ;
#7365 = AXIS2_PLACEMENT_3D ( 'NONE', #11748, #20860, #18868 ) ;
#7366 = ORIENTED_EDGE ( 'NONE', *, *, #6741, .F. ) ;
#7367 = CC_DESIGN_PERSON_AND_ORGANIZATION_ASSIGNMENT ( #13291, #9267, ( #1697 ) ) ;
#7368 = LINE ( 'NONE', #7704, #20581 ) ;
#7369 = DATE_AND_TIME ( #1755, #9596 ) ;
#7370 = DIRECTION ( 'NONE',  ( -0.9730401042858035643, 0.2306359803922028717, 5.958148513035547083E-17 ) ) ;
#7371 = CALENDAR_DATE ( 2026, 31, 10 ) ;
#7372 = DIRECTION ( 'NONE',  ( -0.005235963827121952255, 0.9999862922474493931, -2.738476122049126182E-14 ) ) ;
#7373 = VECTOR ( 'NONE', #9204, 1000.000000000000000 ) ;
#7374 =( LENGTH_UNIT ( ) NAMED_UNIT ( * ) SI_UNIT ( .MILLI., .METRE. ) );
#7375 = CIRCLE ( 'NONE', #2808, 2.458500000000000352 ) ;
#7376 = APPLICATION_PROTOCOL_DEFINITION ( 'international standard', 'config_control_design', 1994, #22467 ) ;
#7377 = ADVANCED_FACE ( 'NONE', ( #21653 ), #6975, .T. ) ;
#7378 = EDGE_LOOP ( 'NONE', ( #8993, #6075, #3083, #2619 ) ) ;
#7379 = CARTESIAN_POINT ( 'NONE',  ( -20.00000000397129796, 22.95208919256900160, 6.500000000004299672 ) ) ;
#7380 = VERTEX_POINT ( 'NONE', #18111 ) ;
#7381 = DIRECTION ( 'NONE',  ( 6.124378941434239724E-17, -2.274246353359159970E-33, 1.000000000000000000 ) ) ;
#7382 = DIRECTION ( 'NONE',  ( 1.187319687680499994E-16, 2.805478249478695031E-20, 1.000000000000000000 ) ) ;
#7383 = FACE_BOUND ( 'NONE', #23335, .T. ) ;
#7384 = EDGE_LOOP ( 'NONE', ( #9045, #22813, #18990, #2138 ) ) ;
#7385 = ORIENTED_EDGE ( 'NONE', *, *, #2567, .F. ) ;
#7386 = CARTESIAN_POINT ( 'NONE',  ( -27.00000000000000000, -31.09999999999999787, 19.00000000000000000 ) ) ;
#7387 = EDGE_LOOP ( 'NONE', ( #19149, #4979, #16475, #10990, #21337 ) ) ;
#7388 = PERSON ( 'NAUO-PER29', 'UNSPECIFIED', 'UNSPECIFIED', ('UNSPECIFIED'), ('UNSPECIFIED'), ('UNSPECIFIED') ) ;
#7389 = ADVANCED_FACE ( 'NONE', ( #5275 ), #13029, .T. ) ;
#7390 = SHAPE_DEFINITION_REPRESENTATION ( #11501, #23243 ) ;
#7392 = ADVANCED_FACE ( 'NONE', ( #17875 ), #20006, .T. ) ;
#7391 = ORIENTED_EDGE ( 'NONE', *, *, #4023, .F. ) ;
#7393 = EDGE_LOOP ( 'NONE', ( #10814, #20976, #17516, #13297 ) ) ;
#7394 = CARTESIAN_POINT ( 'NONE',  ( 113.2033677465029911, -29.17473274740279976, 13.00000000000000000 ) ) ;
#7395 = FACE_OUTER_BOUND ( 'NONE', #15901, .T. ) ;
#7396 = CALENDAR_DATE ( 2026, 31, 10 ) ;
#7397 = DIRECTION ( 'NONE',  ( 1.173102895937339952E-16, 2.365413804416879953E-16, 1.000000000000000000 ) ) ;
#7398 = LINE ( 'NONE', #1789, #16312 ) ;
#7399 = EDGE_LOOP ( 'NONE', ( #15664, #7491, #8183, #3109, #21180 ) ) ;
#7400 = CARTESIAN_POINT ( 'NONE',  ( -20.00000000000000000, -20.00000000000000000, 5.000000000004559908 ) ) ;
#7401 = COORDINATED_UNIVERSAL_TIME_OFFSET ( 0, 0, .AHEAD. ) ;
#7402 = ADVANCED_FACE ( 'NONE', ( #7309 ), #18334, .F. ) ;
#7403 = ORIENTED_EDGE ( 'NONE', *, *, #19511, .T. ) ;
#7404 = CARTESIAN_POINT ( 'NONE',  ( 26.11627841292215280, -8.532812502301570845, 16.00000000000000000 ) ) ;
#7405 = DIRECTION ( 'NONE',  ( -0.005235963827197880234, 0.9999862922474489491, 6.376474323085884347E-17 ) ) ;
#7406 = AXIS2_PLACEMENT_3D ( 'NONE', #20320, #3935, #11209 ) ;
#7407 = DIRECTION ( 'NONE',  ( -3.210834492181135034E-17, 2.441916418604790135E-15, 1.000000000000000000 ) ) ;
#7408 = DIRECTION ( 'NONE',  ( 6.123230199561459225E-17, 4.868008300101910084E-15, 1.000000000000000000 ) ) ;
#7409 = DIRECTION ( 'NONE',  ( -2.982858504577894622E-17, 2.441916418604795262E-15, 1.000000000000000000 ) ) ;
#7410 = ORIENTED_EDGE ( 'NONE', *, *, #14795, .F. ) ;
#7411 = CARTESIAN_POINT ( 'NONE',  ( -17.47493720815189633, 28.95208920939580111, 8.000000000004419576 ) ) ;
#7412 = EDGE_CURVE ( 'NONE', #2200, #8421, #10999, .T. ) ;
#7413 = PRODUCT_DEFINITION_SHAPE ( 'NONE', 'NONE',  #23494 ) ;
#7414 = ORIENTED_EDGE ( 'NONE', *, *, #12692, .F. ) ;
#7415 = LINE ( 'NONE', #21642, #4304 ) ;
#7416 = CARTESIAN_POINT ( 'NONE',  ( 113.4570673249340018, -28.10438863268850085, 3.399999999999999911 ) ) ;
#7417 = ORIENTED_EDGE ( 'NONE', *, *, #22161, .T. ) ;
#7418 = CARTESIAN_POINT ( 'NONE',  ( 36.43025397111700414, 13.30208005948959915, 26.50000000000000000 ) ) ;
#7419 = ORIENTED_EDGE ( 'NONE', *, *, #22588, .F. ) ;
#7420 = AXIS2_PLACEMENT_3D ( 'NONE', #13987, #4843, #17681 ) ;
#7421 = CARTESIAN_POINT ( 'NONE',  ( 46.93847685464109531, -4.150000499290836586, -13.00000000000000000 ) ) ;
#7422 = COORDINATED_UNIVERSAL_TIME_OFFSET ( 0, 0, .AHEAD. ) ;
#7423 = CARTESIAN_POINT ( 'NONE',  ( 33.27705887009690144, -3.036156860537199798, -13.00000000000039968 ) ) ;
#7424 = DIRECTION ( 'NONE',  ( -0.2306359803922066187, -0.9730401042858026761, 0.000000000000000000 ) ) ;
#7425 = CARTESIAN_POINT ( 'NONE',  ( -20.00000000397369959, 22.95208919256949898, -2.500000000000059952 ) ) ;
#7426 = DIRECTION ( 'NONE',  ( 1.000000000000000000, 0.000000000000000000, 0.000000000000000000 ) ) ;
#7427 = DIRECTION ( 'NONE',  ( -0.9730401042858022320, 0.2306359803922080343, 5.959266323858941219E-17 ) ) ;
#7428 = DIRECTION ( 'NONE',  ( 3.210834492181139964E-17, -2.441916418604790135E-15, -1.000000000000000000 ) ) ;
#7429 = CC_DESIGN_PERSON_AND_ORGANIZATION_ASSIGNMENT ( #2182, #3844, ( #11812 ) ) ;
#7430 = CARTESIAN_POINT ( 'NONE',  ( 34.89491389100810181, 23.30074776265910330, -17.25000000000050093 ) ) ;
#7431 = DIRECTION ( 'NONE',  ( 0.000000000000000000, 0.000000000000000000, -1.000000000000000000 ) ) ;
#7432 = LINE ( 'NONE', #3737, #19114 ) ;
#7433 = CARTESIAN_POINT ( 'NONE',  ( -32.64682763696299617, 7.329162855357659545, -3.750000000000000000 ) ) ;
#7434 = ORIENTED_EDGE ( 'NONE', *, *, #8913, .F. ) ;
#7435 = CIRCLE ( 'NONE', #6297, 2.500000000000000000 ) ;
#7436 = VERTEX_POINT ( 'NONE', #14200 ) ;
#7437 = CARTESIAN_POINT ( 'NONE',  ( 38.12041445833288122, 17.39768532946541413, 12.99999999999979927 ) ) ;
#7438 = CARTESIAN_POINT ( 'NONE',  ( -32.65691263631629226, 9.274125246214079965, 3.750000000000000000 ) ) ;
#7439 = ORIENTED_EDGE ( 'NONE', *, *, #6794, .T. ) ;
#7440 = DIRECTION ( 'NONE',  ( 0.000000000000000000, -6.936119456124777094E-16, -1.000000000000000000 ) ) ;
#7441 = EDGE_LOOP ( 'NONE', ( #16614, #17580, #11613, #16671 ) ) ;
#7442 = DIRECTION ( 'NONE',  ( -0.9999862922474492821, -0.005235963827121951387, 1.466966272682004590E-16 ) ) ;
#7443 = MECHANICAL_CONTEXT ( 'NONE', #20492, 'mechanical' ) ;
#7444 = CARTESIAN_POINT ( 'NONE',  ( 36.05743075878378789, 7.755885733951535244, -8.806355889830928874 ) ) ;
#7445 = EDGE_CURVE ( 'NONE', #5643, #13084, #12662, .T. ) ;
#7446 = PERSON_AND_ORGANIZATION_ROLE ( 'classification_officer' ) ;
#7447 = DIRECTION ( 'NONE',  ( -6.662111140531837817E-09, 1.000000000000000000, -2.081668171172169697E-15 ) ) ;
#7448 = VERTEX_POINT ( 'NONE', #19895 ) ;
#7449 = CIRCLE ( 'NONE', #17698, 3.499999999999999112 ) ;
#7450 = CARTESIAN_POINT ( 'NONE',  ( -25.44812980900369936, 25.46511081327010118, 4.999999999999940492 ) ) ;
#7451 = ORIENTED_EDGE ( 'NONE', *, *, #10404, .F. ) ;
#7452 = CARTESIAN_POINT ( 'NONE',  ( -69.83648240813081998, -6.865755409778316221, 5.500000000000099476 ) ) ;
#7453 = EDGE_CURVE ( 'NONE', #20142, #6574, #14548, .T. ) ;
#7454 = EDGE_CURVE ( 'NONE', #5237, #11903, #15969, .T. ) ;
#7455 = VERTEX_POINT ( 'NONE', #21434 ) ;
#7456 = CARTESIAN_POINT ( 'NONE',  ( 5.000000000000000000, -31.09999999999999787, 5.000000000000000000 ) ) ;
#7457 = DIRECTION ( 'NONE',  ( -0.2306359803922010121, -0.9730401042858040084, 0.000000000000000000 ) ) ;
#7458 = CARTESIAN_POINT ( 'NONE',  ( 41.08211621068439712, 11.24883806106539907, -18.89999999999999858 ) ) ;
#7459 = VERTEX_POINT ( 'NONE', #5162 ) ;
#7460 = APPLICATION_CONTEXT ( 'configuration controlled 3d designs of mechanical parts and assemblies' ) ;
#7461 = AXIS2_PLACEMENT_3D ( 'NONE', #11566, #7974, #7227 ) ;
#7462 = PERSON_AND_ORGANIZATION_ROLE ( 'classification_officer' ) ;
#7463 = CIRCLE ( 'NONE', #10513, 2.999765877365279998 ) ;
#7464 = CARTESIAN_POINT ( 'NONE',  ( -29.94694237017910154, 7.343299551231780242, -5.000000000000000000 ) ) ;
#7465 = ORIENTED_EDGE ( 'NONE', *, *, #11879, .T. ) ;
#7466 = CALENDAR_DATE ( 2026, 31, 10 ) ;
#7467 = ORIENTED_EDGE ( 'NONE', *, *, #22139, .T. ) ;
#7468 = ORIENTED_EDGE ( 'NONE', *, *, #8199, .F. ) ;
#7469 = LINE ( 'NONE', #19823, #18718 ) ;
#7470 = PERSON_AND_ORGANIZATION_ROLE ( 'creator' ) ;
#7471 = ADVANCED_FACE ( 'NONE', ( #18223, #10890 ), #12423, .F. ) ;
#7472 = CARTESIAN_POINT ( 'NONE',  ( -69.88753305544580030, 2.884110939634079607, -3.000000000000079936 ) ) ;
#7473 = DATE_TIME_ROLE ( 'classification_date' ) ;
#7474 = CIRCLE ( 'NONE', #15432, 2.700000000000000178 ) ;
#7475 = LINE ( 'NONE', #14708, #6260 ) ;
#7476 = CC_DESIGN_DATE_AND_TIME_ASSIGNMENT ( #730, #13117, ( #17596 ) ) ;
#7477 = CIRCLE ( 'NONE', #16182, 2.009240000000000581 ) ;
#7478 = PRODUCT_RELATED_PRODUCT_CATEGORY ( 'detail', '', ( #10633 ) ) ;
#7479 = CARTESIAN_POINT ( 'NONE',  ( -20.00000000000000000, -20.00000000000000000, -2.500000000000000000 ) ) ;
#7480 = ADVANCED_FACE ( 'NONE', ( #8970 ), #1943, .T. ) ;
#7481 = EDGE_CURVE ( 'NONE', #16195, #199, #13120, .T. ) ;
#7482 = APPROVAL_ROLE ( '' ) ;
#7483 = ORIENTED_EDGE ( 'NONE', *, *, #3286, .T. ) ;
#7484 = CIRCLE ( 'NONE', #11678, 3.499999999999999556 ) ;
#7485 = DIRECTION ( 'NONE',  ( -1.226293361205523864E-15, -4.915326450861021157E-15, -1.000000000000000000 ) ) ;
#7486 = ORIENTED_EDGE ( 'NONE', *, *, #13985, .T. ) ;
#7487 = DIRECTION ( 'NONE',  ( -0.9730401042858024541, 0.2306359803922080898, 5.959266323858942451E-17 ) ) ;
#7488 = CARTESIAN_POINT ( 'NONE',  ( -59.85533902005759899, -24.86725927682059734, -5.000000000000000000 ) ) ;
#7489 = LINE ( 'NONE', #6049, #9211 ) ;
#7490 = AXIS2_PLACEMENT_3D ( 'NONE', #3577, #20061, #7381 ) ;
#7491 = ORIENTED_EDGE ( 'NONE', *, *, #108, .F. ) ;
#7492 = EDGE_LOOP ( 'NONE', ( #13335, #5231, #7177, #1360 ) ) ;
#7493 = DIRECTION ( 'NONE',  ( 0.000000000000000000, 0.000000000000000000, 1.000000000000000000 ) ) ;
#7494 = ORIENTED_EDGE ( 'NONE', *, *, #4762, .F. ) ;
#7495 = APPROVAL_STATUS ( 'not_yet_approved' ) ;
#7496 = VECTOR ( 'NONE', #15751, 1000.000000000000000 ) ;
#7497 = CIRCLE ( 'NONE', #22257, 2.500000000000000000 ) ;
#7498 = ORIENTED_EDGE ( 'NONE', *, *, #18676, .T. ) ;
#7499 = EDGE_LOOP ( 'NONE', ( #22034, #2149, #8225, #9831 ) ) ;
#7500 = CARTESIAN_POINT ( 'NONE',  ( -16.50000000202540207, 1.899127378699219992, 6.750000000004470202 ) ) ;
#7501 = FACE_OUTER_BOUND ( 'NONE', #13056, .T. ) ;
#7502 = CALENDAR_DATE ( 2026, 31, 10 ) ;
#7503 = CARTESIAN_POINT ( 'NONE',  ( -20.00000000397270128, 22.95208919256889857, -5.499999999995559996 ) ) ;
#7504 = ADVANCED_FACE ( 'NONE', ( #22353 ), #21031, .F. ) ;
#7505 = CARTESIAN_POINT ( 'NONE',  ( -14.70588235717489844, 25.77561860482770228, 8.000000000004400036 ) ) ;
#7506 = CC_DESIGN_DATE_AND_TIME_ASSIGNMENT ( #3085, #21027, ( #5001 ) ) ;
#7507 = CC_DESIGN_PERSON_AND_ORGANIZATION_ASSIGNMENT ( #12126, #8560, ( #12572 ) ) ;
#7508 = SHAPE_REPRESENTATION ( 'Pin 2', ( #12739 ), #21233 ) ;
#7509 = CIRCLE ( 'NONE', #23406, 2.500000000000000000 ) ;
#7510 = EDGE_CURVE ( 'NONE', #3305, #21263, #20468, .T. ) ;
#7511 = EDGE_CURVE ( 'NONE', #16051, #13630, #4298, .T. ) ;
#7512 = ORIENTED_EDGE ( 'NONE', *, *, #20585, .T. ) ;
#7514 = CARTESIAN_POINT ( 'NONE',  ( -20.00000000000000000, -20.00000000000000000, -5.499999999995469402 ) ) ;
#7513 = AXIS2_PLACEMENT_3D ( 'NONE', #7776, #8248, #1333 ) ;
#7515 = APPROVAL_STATUS ( 'not_yet_approved' ) ;
#7516 = CIRCLE ( 'NONE', #15452, 0.0009999999999975306419 ) ;
#7517 = ORIENTED_EDGE ( 'NONE', *, *, #1837, .T. ) ;
#7518 = CARTESIAN_POINT ( 'NONE',  ( -59.85533902005759899, -24.86725927682059734, 5.000000000000000000 ) ) ;
#7519 = CARTESIAN_POINT ( 'NONE',  ( -19.81505072009858992, 25.44523855881121577, -5.499999999995565325 ) ) ;
#7520 = FACE_OUTER_BOUND ( 'NONE', #8001, .T. ) ;
#7521 = DIRECTION ( 'NONE',  ( 0.9730401042858033422, -0.2306359803922031215, 3.994774879569051239E-16 ) ) ;
#7522 = CARTESIAN_POINT ( 'NONE',  ( -26.00000000000149925, -20.00000000055539928, -5.499999999994109601 ) ) ;
#7523 = ORIENTED_EDGE ( 'NONE', *, *, #6654, .T. ) ;
#7524 = CARTESIAN_POINT ( 'NONE',  ( 33.61414435712650572, 10.38347584602063911, 9.000012045631683222 ) ) ;
#7525 = UNCERTAINTY_MEASURE_WITH_UNIT (LENGTH_MEASURE( 1.000000000000000082E-05 ), #17598, 'distance_accuracy_value', 'NONE');
#7526 = ORIENTED_EDGE ( 'NONE', *, *, #11377, .T. ) ;
#7527 = ORIENTED_EDGE ( 'NONE', *, *, #2107, .T. ) ;
#7528 = DIRECTION ( 'NONE',  ( -0.9730401042858022320, 0.2306359803922080343, 5.959266323858941219E-17 ) ) ;
#7529 = FACE_BOUND ( 'NONE', #10320, .T. ) ;
#7530 = ORIENTED_EDGE ( 'NONE', *, *, #14770, .F. ) ;
#7531 = CARTESIAN_POINT ( 'NONE',  ( 88.98991518642344545, 7.652622273256539209, -13.00000000000030020 ) ) ;
#7533 = VERTEX_POINT ( 'NONE', #6548 ) ;
#7532 = ADVANCED_FACE ( 'NONE', ( #11477 ), #12999, .F. ) ;
#7534 = LINE ( 'NONE', #7421, #10536 ) ;
#7535 = AXIS2_PLACEMENT_3D ( 'NONE', #2654, #6448, #13825 ) ;
#7536 = CARTESIAN_POINT ( 'NONE',  ( 37.67179450110460692, -4.077824265976569329, -13.00000000000000000 ) ) ;
#7537 = DIRECTION ( 'NONE',  ( 6.123230199561429643E-17, 4.868008300101910084E-15, 1.000000000000000000 ) ) ;
#7538 = ADVANCED_FACE ( 'NONE', ( #19249 ), #13796, .T. ) ;
#7539 = DIRECTION ( 'NONE',  ( -1.466984912809909902E-16, -2.805478249466335375E-20, -1.000000000000000000 ) ) ;
#7540 = PERSON_AND_ORGANIZATION_ROLE ( 'classification_officer' ) ;
#7541 = ADVANCED_FACE ( 'NONE', ( #2299 ), #4759, .F. ) ;
#7542 = DIRECTION ( 'NONE',  ( -3.099353312215989243E-62, 1.001855809244433740E-92, 1.000000000000000000 ) ) ;
#7543 = PLANE ( 'NONE',  #8279 ) ;
#7544 = CARTESIAN_POINT ( 'NONE',  ( 35.59419854219520118, 9.774809681453278998, -26.30000000000050164 ) ) ;
#7545 = CARTESIAN_POINT ( 'NONE',  ( -1.262685242559879909E-14, -17.30000000000000071, 2.500000000000000000 ) ) ;
#7546 = CLOSED_SHELL ( 'NONE', ( #18101, #12327, #16780, #2971, #1284, #8048 ) ) ;
#7547 = CIRCLE ( 'NONE', #16254, 4.399999999999997691 ) ;
#7548 = CARTESIAN_POINT ( 'NONE',  ( -22.50000000000000000, -20.00000000000000000, -5.000000000000000000 ) ) ;
#7549 = CARTESIAN_POINT ( 'NONE',  ( -59.87132660632070014, -21.81388311970430038, -5.000000000000000000 ) ) ;
#7550 = VERTEX_POINT ( 'NONE', #16789 ) ;
#7551 = VERTEX_POINT ( 'NONE', #16903 ) ;
#7552 = DIRECTION ( 'NONE',  ( -2.269747459788994803E-13, -2.220446049250320181E-15, -1.000000000000000000 ) ) ;
#7553 = DIRECTION ( 'NONE',  ( 1.226293361205523864E-15, 4.915326450861021157E-15, 1.000000000000000000 ) ) ;
#7554 = VERTEX_POINT ( 'NONE', #8321 ) ;
#7555 = CIRCLE ( 'NONE', #11420, 0.1000000000000028644 ) ;
#7556 = CARTESIAN_POINT ( 'NONE',  ( 2.500000000000000000, -31.09999999999999787, -19.00000000000000000 ) ) ;
#7557 = EDGE_LOOP ( 'NONE', ( #314, #5236, #20865, #9390 ) ) ;
#7558 = CARTESIAN_POINT ( 'NONE',  ( 41.15130700480209924, 11.54075009235119964, 15.50000000000000000 ) ) ;
#7559 = APPROVAL_ROLE ( '' ) ;
#7560 = DIRECTION ( 'NONE',  ( 0.000000000000000000, 1.000000000000000000, 0.000000000000000000 ) ) ;
#7561 = CC_DESIGN_PERSON_AND_ORGANIZATION_ASSIGNMENT ( #13323, #9292, ( #11077 ) ) ;
#7562 = LINE ( 'NONE', #9340, #7053 ) ;
#7563 = ORIENTED_EDGE ( 'NONE', *, *, #3881, .F. ) ;
#7564 = LOCAL_TIME ( 14, 11, 27.00000000000000000, #9136 ) ;
#7565 = CARTESIAN_POINT ( 'NONE',  ( 6.500000000000000000, 0.000000000000000000, -2.500000000000000000 ) ) ;
#7566 = ORIENTED_EDGE ( 'NONE', *, *, #7751, .T. ) ;
#7567 = PLANE ( 'NONE',  #20001 ) ;
#7568 = DIRECTION ( 'NONE',  ( -0.2306359803922053142, -0.9730401042858028982, 0.000000000000000000 ) ) ;
#7569 = ORIENTED_EDGE ( 'NONE', *, *, #20297, .T. ) ;
#7570 = CARTESIAN_POINT ( 'NONE',  ( -12.50000000434259917, 26.95208919326709918, 6.750000000004369838 ) ) ;
#7571 = DIRECTION ( 'NONE',  ( 1.133739489558799860E-16, 7.703614176864520825E-35, 1.000000000000000000 ) ) ;
#7572 = FACE_BOUND ( 'NONE', #15168, .T. ) ;
#7573 = VERTEX_POINT ( 'NONE', #7887 ) ;
#7574 = ADVANCED_FACE ( 'NONE', ( #2537 ), #15118, .T. ) ;
#7575 = SECURITY_CLASSIFICATION_LEVEL ( 'unclassified' ) ;
#7576 = DIRECTION ( 'NONE',  ( 6.123237831918399306E-17, -1.569224110909209817E-30, -1.000000000000000000 ) ) ;
#7577 = ORIENTED_EDGE ( 'NONE', *, *, #20084, .T. ) ;
#7578 = APPROVAL_ROLE ( '' ) ;
#7579 = DIRECTION ( 'NONE',  ( 1.169815979547696263E-44, 1.000000000000000000, 5.153216234642169651E-30 ) ) ;
#7580 = ORIENTED_EDGE ( 'NONE', *, *, #11565, .F. ) ;
#7581 = VERTEX_POINT ( 'NONE', #11601 ) ;
#7582 = CARTESIAN_POINT ( 'NONE',  ( 62.31663085210120556, 16.28722946541822836, 3.908114637620867245E-14 ) ) ;
#7583 = SECURITY_CLASSIFICATION_LEVEL ( 'unclassified' ) ;
#7584 = VECTOR ( 'NONE', #23389, 1000.000000000000114 ) ;
#7585 = CARTESIAN_POINT ( 'NONE',  ( -14.00000000397430000, 22.95208919312840123, -6.749999999996930455 ) ) ;
#7586 = CALENDAR_DATE ( 2026, 31, 10 ) ;
#7587 = DIRECTION ( 'NONE',  ( 0.9730401042858024541, -0.2306359803922080898, -5.959266323858942451E-17 ) ) ;
#7588 = DIRECTION ( 'NONE',  ( -0.2306359803922028995, -0.9730401042858036753, 5.121148285185918258E-15 ) ) ;
#7589 = DATE_AND_TIME ( #1882, #15934 ) ;
#7590 = PRODUCT_DEFINITION_SHAPE ( 'NONE', 'NONE',  #23489 ) ;
#7591 = LOCAL_TIME ( 14, 11, 27.00000000000000000, #2721 ) ;
#7592 = EDGE_LOOP ( 'NONE', ( #11467, #18977, #912, #20480, #16499 ) ) ;
#7593 = CARTESIAN_POINT ( 'NONE',  ( 35.09747506357100377, 11.43410645592859964, 29.25000000000000000 ) ) ;
#7594 = ORIENTED_EDGE ( 'NONE', *, *, #12184, .F. ) ;
#7595 = VECTOR ( 'NONE', #1959, 1000.000000000000000 ) ;
#7596 = ADVANCED_FACE ( 'NONE', ( #515 ), #8863, .F. ) ;
#7597 = FACE_OUTER_BOUND ( 'NONE', #2085, .T. ) ;
#7598 = CARTESIAN_POINT ( 'NONE',  ( -19.52710366811739817, 1.147603427694289913, -5.000000000000000000 ) ) ;
#7599 = CARTESIAN_POINT ( 'NONE',  ( 35.59419854219520118, 9.774809681453550780, 26.68999999999999773 ) ) ;
#7600 = EDGE_LOOP ( 'NONE', ( #6280, #16640, #14563, #14744 ) ) ;
#7601 = ORIENTED_EDGE ( 'NONE', *, *, #22108, .T. ) ;
#7602 = DIRECTION ( 'NONE',  ( -0.9997648975362233292, -0.02168293463497958373, 0.000000000000000000 ) ) ;
#7603 = EDGE_LOOP ( 'NONE', ( #13785, #9118, #12494, #20839 ) ) ;
#7604 = CC_DESIGN_DATE_AND_TIME_ASSIGNMENT ( #4481, #19100, ( #1214 ) ) ;
#7605 = DATE_AND_TIME ( #20316, #8756 ) ;
#7606 = EDGE_LOOP ( 'NONE', ( #14646, #4624 ) ) ;
#7607 = ORIENTED_EDGE ( 'NONE', *, *, #14997, .F. ) ;
#7608 = CARTESIAN_POINT ( 'NONE',  ( -62.74088165156670271, -25.10566213532069924, -5.538319619822460249E-15 ) ) ;
#7609 = VECTOR ( 'NONE', #19973, 1000.000000000000227 ) ;
#7610 = DATE_AND_TIME ( #17969, #1583 ) ;
#7611 = ADVANCED_FACE ( 'NONE', ( #22005 ), #1059, .T. ) ;
#7612 = CARTESIAN_POINT ( 'NONE',  ( -20.00000000000000000, -20.00000000000000000, -2.500000000000000000 ) ) ;
#7613 = EDGE_CURVE ( 'NONE', #11939, #2591, #11239, .T. ) ;
#7614 = PRODUCT_DEFINITION_FORMATION_WITH_SPECIFIED_SOURCE ( 'ANY', '', #21422, .NOT_KNOWN. ) ;
#7615 = CARTESIAN_POINT ( 'NONE',  ( 102.8131131701580046, 7.202356331284469171, -13.00000000000000000 ) ) ;
#7616 = SECURITY_CLASSIFICATION ( '', '', #735 ) ;
#7617 = ORIENTED_EDGE ( 'NONE', *, *, #22186, .F. ) ;
#7618 = CARTESIAN_POINT ( 'NONE',  ( 38.19845176233020823, -1.855887187839940777, -13.00000000000000000 ) ) ;
#7619 = SHAPE_DEFINITION_REPRESENTATION ( #8918, #2509 ) ;
#7620 = ORIENTED_EDGE ( 'NONE', *, *, #7210, .F. ) ;
#7621 = DIRECTION ( 'NONE',  ( 0.9730401042858035643, -0.2306359803922028717, 2.804983810440357815E-16 ) ) ;
#7622 = CARTESIAN_POINT ( 'NONE',  ( 28.54501609403209983, -1.321191992434479934, -15.00000000000039968 ) ) ;
#7623 = EDGE_CURVE ( 'NONE', #2498, #17128, #6589, .T. ) ;
#7624 = PRODUCT_DEFINITION_FORMATION_WITH_SPECIFIED_SOURCE ( 'ANY', '', #11960, .NOT_KNOWN. ) ;
#7625 = CARTESIAN_POINT ( 'NONE',  ( 69.48351927594264055, 14.58848926887901065, 1.155720087641903136E-14 ) ) ;
#7626 = DIRECTION ( 'NONE',  ( -0.005235963827101446089, 0.9999862922474493931, 7.400535959109775519E-19 ) ) ;
#7627 = CC_DESIGN_SECURITY_CLASSIFICATION ( #8771, ( #796 ) ) ;
#7628 = EDGE_LOOP ( 'NONE', ( #4847, #12910, #11490, #8549 ) ) ;
#7629 = DIRECTION ( 'NONE',  ( 0.9730401042858022320, -0.2306359803922080343, 1.063156381331940328E-15 ) ) ;
#7630 = CC_DESIGN_PERSON_AND_ORGANIZATION_ASSIGNMENT ( #8267, #12194, ( #5063 ) ) ;
#7631 = ORIENTED_EDGE ( 'NONE', *, *, #2134, .T. ) ;
#7632 = CC_DESIGN_PERSON_AND_ORGANIZATION_ASSIGNMENT ( #6634, #21099, ( #16771 ) ) ;
#7633 = VERTEX_POINT ( 'NONE', #22126 ) ;
#7634 = CARTESIAN_POINT ( 'NONE',  ( 41.17437060284130013, 11.63805410277969976, -19.59999999999999787 ) ) ;
#7635 = CARTESIAN_POINT ( 'NONE',  ( -32.64674982798959491, 7.329300507370480666, 5.000000000000000000 ) ) ;
#7636 = ORGANIZATION ( 'NAUO-ORG14', 'UNSPECIFIED', 'UNSPECIFIED' ) ;
#7637 =( REPRESENTATION_RELATIONSHIP ('NONE','NONE', #18771, #23243 ) REPRESENTATION_RELATIONSHIP_WITH_TRANSFORMATION ( #9555 )SHAPE_REPRESENTATION_RELATIONSHIP( ) );
#7638 = ORIENTED_EDGE ( 'NONE', *, *, #11942, .F. ) ;
#7639 = EDGE_CURVE ( 'NONE', #5148, #18943, #5871, .T. ) ;
#7640 = DIRECTION ( 'NONE',  ( 0.2306359803922025387, 0.9730401042858035643, -4.741332172907917461E-18 ) ) ;
#7641 = EDGE_CURVE ( 'NONE', #18815, #15778, #19861, .T. ) ;
#7642 = PERSON ( 'NAUO-PER36', 'UNSPECIFIED', 'UNSPECIFIED', ('UNSPECIFIED'), ('UNSPECIFIED'), ('UNSPECIFIED') ) ;
#7643 = CC_DESIGN_PERSON_AND_ORGANIZATION_ASSIGNMENT ( #17835, #21395, ( #19552 ) ) ;
#7644 = DIRECTION ( 'NONE',  ( 1.000000000000000000, -1.213490492418610097E-15, 0.000000000000000000 ) ) ;
#7645 = ITEM_DEFINED_TRANSFORMATION ( 'NONE', 'NONE', #7234,  #12739 ) ;
#7646 = LINE ( 'NONE', #16431, #16574 ) ;
#7647 = CC_DESIGN_APPROVAL ( #12304, ( #14088 ) ) ;
#7648 = AXIS2_PLACEMENT_3D ( 'NONE', #10102, #22902, #13769 ) ;
#7649 = CARTESIAN_POINT ( 'NONE',  ( -20.00000000000000000, -20.00000000000000000, -5.000000000000000000 ) ) ;
#7650 = CARTESIAN_POINT ( 'NONE',  ( -22.75000000000231637, -20.00000000000000000, -8.499999999994834354 ) ) ;
#7651 = DATE_AND_TIME ( #18828, #22402 ) ;
#7652 = CARTESIAN_POINT ( 'NONE',  ( 43.87899317387989839, 21.17128575569940097, 13.00000000000000000 ) ) ;
#7653 = LINE ( 'NONE', #18589, #16834 ) ;
#7654 = LINE ( 'NONE', #17024, #5232 ) ;
#7655 = DIRECTION ( 'NONE',  ( 1.000000000000000000, -2.269747459789000104E-13, -7.174648137343060814E-44 ) ) ;
#7656 = EDGE_CURVE ( 'NONE', #21726, #9182, #13235, .T. ) ;
#7657 = LINE ( 'NONE', #2660, #2709 ) ;
#7658 = DIRECTION ( 'NONE',  ( -0.9730401042858036753, 0.2306359803922031493, 5.432877459303543355E-17 ) ) ;
#7659 = LINE ( 'NONE', #2663, #6566 ) ;
#7660 = VERTEX_POINT ( 'NONE', #3211 ) ;
#7661 = PRODUCT_DEFINITION_FORMATION_WITH_SPECIFIED_SOURCE ( 'ANY', '', #576, .NOT_KNOWN. ) ;
#7662 = ORIENTED_EDGE ( 'NONE', *, *, #15469, .F. ) ;
#7663 = CARTESIAN_POINT ( 'NONE',  ( -2.500000000000000000, 0.000000000000000000, -2.500000000000000000 ) ) ;
#7664 = CARTESIAN_POINT ( 'NONE',  ( 37.10730959030829723, 23.96304573415810069, -15.00000000000049916 ) ) ;
#7665 = VERTEX_POINT ( 'NONE', #14013 ) ;
#7666 = CIRCLE ( 'NONE', #4240, 2.066999999999999282 ) ;
#7667 = EDGE_CURVE ( 'NONE', #2112, #20086, #8449, .T. ) ;
#7668 = DIRECTION ( 'NONE',  ( 1.000000000000000000, 0.000000000000000000, 0.000000000000000000 ) ) ;
#7669 = ORIENTED_EDGE ( 'NONE', *, *, #10647, .T. ) ;
#7670 = EDGE_CURVE ( 'NONE', #15793, #19671, #22881, .T. ) ;
#7671 = LINE ( 'NONE', #2086, #5303 ) ;
#7672 = LOCAL_TIME ( 14, 11, 27.00000000000000000, #4243 ) ;
#7673 = DATE_AND_TIME ( #6008, #1619 ) ;
#7674 = CARTESIAN_POINT ( 'NONE',  ( 36.69831606175046090, 11.52739241660666814, -8.784148981162500647 ) ) ;
#7675 = AXIS2_PLACEMENT_3D ( 'NONE', #13561, #2278, #3954 ) ;
#7676 = APPROVAL_STATUS ( 'not_yet_approved' ) ;
#7677 = CIRCLE ( 'NONE', #3875, 2.500000000000000000 ) ;
#7678 = FACE_OUTER_BOUND ( 'NONE', #11229, .T. ) ;
#7679 = ORIENTED_EDGE ( 'NONE', *, *, #8835, .T. ) ;
#7680 = CC_DESIGN_APPROVAL ( #8661, ( #17927 ) ) ;
#7681 = CARTESIAN_POINT ( 'NONE',  ( 31.01827548281339375, -2.500766059351008153, 15.00000000000011369 ) ) ;
#7682 = AXIS2_PLACEMENT_3D ( 'NONE', #18451, #9893, #20335 ) ;
#7683 = ORIENTED_EDGE ( 'NONE', *, *, #10217, .T. ) ;
#7684 = CARTESIAN_POINT ( 'NONE',  ( -26.68881687192900287, -6.639832696913689603, -2.500292893218899692 ) ) ;
#7685 = AXIS2_PLACEMENT_3D ( 'NONE', #19787, #14435, #12552 ) ;
#7686 = AXIS2_PLACEMENT_3D ( 'NONE', #22255, #2672, #2451 ) ;
#7687 = DIRECTION ( 'NONE',  ( -3.099353312215988811E-62, -9.818186930595456717E-93, 1.000000000000000000 ) ) ;
#7688 = VERTEX_POINT ( 'NONE', #22921 ) ;
#7689 = DIRECTION ( 'NONE',  ( -0.9730401042858035643, 0.2306359803922028717, 5.958148513035547083E-17 ) ) ;
#7690 = CARTESIAN_POINT ( 'NONE',  ( 36.17078849317571354, 12.20740994216786746, -10.99076000000051145 ) ) ;
#7691 = FACE_OUTER_BOUND ( 'NONE', #1434, .T. ) ;
#7692 = ORIENTED_EDGE ( 'NONE', *, *, #19736, .F. ) ;
#7693 = AXIS2_PLACEMENT_3D ( 'NONE', #10516, #6460, #21179 ) ;
#7694 = DATE_AND_TIME ( #18513, #9966 ) ;
#7695 = CYLINDRICAL_SURFACE ( 'NONE', #2358, 3.500000000000001332 ) ;
#7696 = EDGE_CURVE ( 'NONE', #23387, #16843, #21594, .T. ) ;
#7697 = VECTOR ( 'NONE', #18250, 1000.000000000000000 ) ;
#7698 = ORIENTED_EDGE ( 'NONE', *, *, #2304, .T. ) ;
#7699 = COORDINATED_UNIVERSAL_TIME_OFFSET ( 0, 0, .AHEAD. ) ;
#7700 = DIRECTION ( 'NONE',  ( 2.270069654138870255E-15, 1.000000000000000000, 7.035747901516317327E-77 ) ) ;
#7701 = CC_DESIGN_APPROVAL ( #18224, ( #17948 ) ) ;
#7702 = ORIENTED_EDGE ( 'NONE', *, *, #20211, .F. ) ;
#7703 = VERTEX_POINT ( 'NONE', #17599 ) ;
#7704 = CARTESIAN_POINT ( 'NONE',  ( -13.66074082773489984, 1.277408929928570025, 3.750000000000000000 ) ) ;
#7705 = APPROVAL_ROLE ( '' ) ;
#7706 = CIRCLE ( 'NONE', #8853, 2.749999999999999112 ) ;
#7707 = VECTOR ( 'NONE', #7528, 1000.000000000000227 ) ;
#7708 = AXIS2_PLACEMENT_3D ( 'NONE', #7418, #18462, #1931 ) ;
#7709 = APPROVAL_DATE_TIME ( #2713, #5292 ) ;
#7710 = CARTESIAN_POINT ( 'NONE',  ( 54.98564867634340203, -10.30593110903627441, 13.00000000000000000 ) ) ;
#7711 = ADVANCED_FACE ( 'NONE', ( #3325 ), #16031, .F. ) ;
#7712 = SHAPE_REPRESENTATION_RELATIONSHIP ( 'NONE' , 'NONE' ,  #1107, #12489 ) ;
#7714 = AXIS2_PLACEMENT_3D ( 'NONE', #6097, #22798, #18586 ) ;
#7713 = CARTESIAN_POINT ( 'NONE',  ( -68.53146193154570653, -21.85922789657999843, -2.680796741387739937E-15 ) ) ;
#7715 = COORDINATED_UNIVERSAL_TIME_OFFSET ( 0, 0, .AHEAD. ) ;
#7716 = LOCAL_TIME ( 14, 11, 27.00000000000000000, #18350 ) ;
#7717 = CIRCLE ( 'NONE', #11921, 3.499999999999999556 ) ;
#7718 = VERTEX_POINT ( 'NONE', #1304 ) ;
#7719 = CIRCLE ( 'NONE', #13035, 3.750000000000000000 ) ;
#7720 = CARTESIAN_POINT ( 'NONE',  ( 45.07211867146829576, 28.08243186520860135, 19.99999999999969802 ) ) ;
#7721 = EDGE_LOOP ( 'NONE', ( #12786, #17050 ) ) ;
#7722 = CARTESIAN_POINT ( 'NONE',  ( 114.8178196092480050, -22.36345201740219935, -13.00000000000000000 ) ) ;
#7723 = CIRCLE ( 'NONE', #16758, 2.500999999999919954 ) ;
#7724 = LINE ( 'NONE', #22075, #5844 ) ;
#7725 = FACE_OUTER_BOUND ( 'NONE', #14107, .T. ) ;
#7726 = ORIENTED_EDGE ( 'NONE', *, *, #17709, .F. ) ;
#7727 = ORIENTED_EDGE ( 'NONE', *, *, #16600, .F. ) ;
#7728 = DIRECTION ( 'NONE',  ( -0.005235963827108352890, 0.9999862922474493931, 5.936218956694023463E-19 ) ) ;
#7729 = ORIENTED_EDGE ( 'NONE', *, *, #7641, .T. ) ;
#7730 = PERSON_AND_ORGANIZATION_ROLE ( 'creator' ) ;
#7731 = ORIENTED_EDGE ( 'NONE', *, *, #22977, .F. ) ;
#7732 = EDGE_LOOP ( 'NONE', ( #5054, #10935, #9902, #9327 ) ) ;
#7733 = LINE ( 'NONE', #20319, #6213 ) ;
#7734 = DIRECTION ( 'NONE',  ( -1.000000000000000000, 0.000000000000000000, 0.000000000000000000 ) ) ;
#7735 = CALENDAR_DATE ( 2026, 31, 10 ) ;
#7736 = DIRECTION ( 'NONE',  ( -1.000000000000000000, -6.662111140531837817E-09, 1.110223024625157172E-14 ) ) ;
#7737 = AXIS2_PLACEMENT_3D ( 'NONE', #10537, #15974, #15507 ) ;
#7738 = FACE_OUTER_BOUND ( 'NONE', #2446, .T. ) ;
#7739 = AXIS2_PLACEMENT_3D ( 'NONE', #18889, #4393, #6290 ) ;
#7740 = EDGE_CURVE ( 'NONE', #9304, #2112, #15687, .T. ) ;
#7741 = EDGE_CURVE ( 'NONE', #17836, #13324, #1418, .T. ) ;
#7742 = CC_DESIGN_PERSON_AND_ORGANIZATION_ASSIGNMENT ( #5180, #19438, ( #17878 ) ) ;
#7743 = ORIENTED_EDGE ( 'NONE', *, *, #6646, .F. ) ;
#7744 = DIRECTION ( 'NONE',  ( 2.269747459789000104E-13, 2.220446049250330436E-15, 1.000000000000000000 ) ) ;
#7745 = DATE_TIME_ROLE ( 'classification_date' ) ;
#7746 = ORIENTED_EDGE ( 'NONE', *, *, #4086, .T. ) ;
#7747 = DIRECTION ( 'NONE',  ( 0.2306359803922031215, 0.9730401042858035643, 4.620383928407073520E-16 ) ) ;
#7748 = CARTESIAN_POINT ( 'NONE',  ( -27.00000000000000000, -31.09999999999999787, 21.50000000000000000 ) ) ;
#7749 = ORIENTED_EDGE ( 'NONE', *, *, #15354, .T. ) ;
#7750 = EDGE_CURVE ( 'NONE', #142, #3422, #1181, .T. ) ;
#7751 = EDGE_CURVE ( 'NONE', #2368, #23420, #1529, .T. ) ;
#7752 = DIRECTION ( 'NONE',  ( -0.6880432561069586006, 0.1630842657209346236, 0.7071067811865459074 ) ) ;
#7753 = CARTESIAN_POINT ( 'NONE',  ( -17.47493720815390006, 28.95208920939580111, -7.999999999996148858 ) ) ;
#7754 = ORIENTED_EDGE ( 'NONE', *, *, #16581, .T. ) ;
#7755 = CARTESIAN_POINT ( 'NONE',  ( 114.1489752661110089, -25.18526831983109915, -3.000000000000000000 ) ) ;
#7756 = PERSON_AND_ORGANIZATION ( #11966, #8758 ) ;
#7757 = ORIENTED_EDGE ( 'NONE', *, *, #18352, .F. ) ;
#7758 = VERTEX_POINT ( 'NONE', #15692 ) ;
#7759 = DIRECTION ( 'NONE',  ( 0.9730401042858024541, -0.2306359803922080898, -5.959266323853532591E-17 ) ) ;
#7760 = DIRECTION ( 'NONE',  ( -0.9730401042858034533, 0.2306359803922031215, 0.000000000000000000 ) ) ;
#7761 = ORIENTED_EDGE ( 'NONE', *, *, #18976, .F. ) ;
#7762 = APPLICATION_PROTOCOL_DEFINITION ( 'international standard', 'config_control_design', 1994, #6565 ) ;
#7763 = DIRECTION ( 'NONE',  ( 0.6862566701892789389, 0.7273594590164639273, -3.657607522630180133E-15 ) ) ;
#7764 = DIRECTION ( 'NONE',  ( 0.000000000000000000, 0.000000000000000000, 1.000000000000000000 ) ) ;
#7765 = APPROVAL_STATUS ( 'not_yet_approved' ) ;
#7766 = CARTESIAN_POINT ( 'NONE',  ( 114.1489752661110089, -25.18526831983100323, -3.400000000000049649 ) ) ;
#7767 = EDGE_CURVE ( 'NONE', #8933, #1694, #22863, .T. ) ;
#7768 = APPLICATION_CONTEXT ( 'configuration controlled 3d designs of mechanical parts and assemblies' ) ;
#7769 = DIRECTION ( 'NONE',  ( -0.1630842657209323754, -0.6880432561069493858, 0.7071067811865554553 ) ) ;
#7770 = CIRCLE ( 'NONE', #9689, 0.5000000000000004441 ) ;
#7771 = CC_DESIGN_PERSON_AND_ORGANIZATION_ASSIGNMENT ( #442, #5921, ( #3831 ) ) ;
#7772 = DIRECTION ( 'NONE',  ( -3.210834492194344756E-17, 2.441916418604790135E-15, 1.000000000000000000 ) ) ;
#7773 = PERSON_AND_ORGANIZATION ( #11966, #8758 ) ;
#7774 = CC_DESIGN_PERSON_AND_ORGANIZATION_ASSIGNMENT ( #22345, #6091, ( #22038 ) ) ;
#7775 = DIRECTION ( 'NONE',  ( 1.000000000000000000, -3.416070845000479880E-16, 0.000000000000000000 ) ) ;
#7776 = CARTESIAN_POINT ( 'NONE',  ( -12.33340651292470014, 21.13490689743859718, -3.289309883929029635E-15 ) ) ;
#7777 = EDGE_CURVE ( 'NONE', #11668, #12386, #16108, .T. ) ;
#7778 = ADVANCED_FACE ( 'NONE', ( #8916 ), #6905, .F. ) ;
#7779 = FACE_BOUND ( 'NONE', #19444, .T. ) ;
#7780 = CARTESIAN_POINT ( 'NONE',  ( 35.84667945578129888, -10.83917230622230043, 3.100000000000039613 ) ) ;
#7781 = DIRECTION ( 'NONE',  ( 0.9822591002358885826, -0.1875288244611549582, 5.059610138265688673E-16 ) ) ;
#7782 = CARTESIAN_POINT ( 'NONE',  ( 34.94102482032229773, 25.66320561742200113, -13.00000000000049916 ) ) ;
#7783 = ORIENTED_EDGE ( 'NONE', *, *, #6373, .T. ) ;
#7784 = AXIS2_PLACEMENT_3D ( 'NONE', #5023, #18287, #4903 ) ;
#7785 = ORIENTED_EDGE ( 'NONE', *, *, #15908, .T. ) ;
#7786 = DIRECTION ( 'NONE',  ( 1.000000000000000000, 2.982858504577319616E-17, 8.758115402030109610E-48 ) ) ;
#7787 =( BOUNDED_CURVE ( )  B_SPLINE_CURVE ( 2, ( #6716, #3015, #15609 ),
 .UNSPECIFIED., .F., .T. ) 
 B_SPLINE_CURVE_WITH_KNOTS ( ( 3, 3 ),
 ( 0.000000000000000000, 0.2336872276155859962 ),
 .UNSPECIFIED. ) 
 CURVE ( )  GEOMETRIC_REPRESENTATION_ITEM ( )  RATIONAL_B_SPLINE_CURVE ( ( 1.000000000000000000, 1.154700538379259900, 1.000000000000000000 ) ) 
 REPRESENTATION_ITEM ( '' )  );
#7788 = DIRECTION ( 'NONE',  ( -4.028143194477080210E-16, -2.054129435991050111E-15, -1.000000000000000000 ) ) ;
#7789 = ORIENTED_EDGE ( 'NONE', *, *, #2710, .T. ) ;
#7790 = DIRECTION ( 'NONE',  ( -2.269747459788994803E-13, -2.220446049250325308E-15, -1.000000000000000000 ) ) ;
#7791 = EDGE_LOOP ( 'NONE', ( #18057, #4281, #11232, #3835, #18872 ) ) ;
#7792 = CARTESIAN_POINT ( 'NONE',  ( -17.00058775598304095, -0.04789535763852828532, -2.500000000000000000 ) ) ;
#7793 = APPROVAL_DATE_TIME ( #292, #14736 ) ;
#7794 = CARTESIAN_POINT ( 'NONE',  ( 37.54227681792503546, 9.031923193207390455, -8.999975802806220671 ) ) ;
#7795 = ADVANCED_FACE ( 'NONE', ( #10238, #4877, #21485, #14364, #8681, #5224 ), #17462, .T. ) ;
#7796 = PRODUCT ( '1602p_c_03', '1602p_c_03', '', ( #7443 ) ) ;
#7797 = COORDINATED_UNIVERSAL_TIME_OFFSET ( 0, 0, .AHEAD. ) ;
#7798 = CARTESIAN_POINT ( 'NONE',  ( -26.75617730459320143, 6.359992804688050505, 2.500999999999740098 ) ) ;
#7799 = DIRECTION ( 'NONE',  ( 0.9730401042858035643, -0.2306359803922028717, 2.740969466505749044E-16 ) ) ;
#7800 = ORIENTED_EDGE ( 'NONE', *, *, #8995, .T. ) ;
#7801 =( GEOMETRIC_REPRESENTATION_CONTEXT ( 3 ) GLOBAL_UNCERTAINTY_ASSIGNED_CONTEXT ( ( #15284 ) ) GLOBAL_UNIT_ASSIGNED_CONTEXT ( ( #8516, #2683, #13497 ) ) REPRESENTATION_CONTEXT ( 'NONE', 'WORKASPACE' ) );
#7802 = DIRECTION ( 'NONE',  ( -6.281952996264290168E-17, -4.969341027148640384E-15, -1.000000000000000000 ) ) ;
#7803 = VERTEX_POINT ( 'NONE', #19364 ) ;
#7804 = CARTESIAN_POINT ( 'NONE',  ( 35.59419854219520118, 9.774809681453278998, -21.50000000000000000 ) ) ;
#7805 = EDGE_CURVE ( 'NONE', #19990, #16463, #3093, .T. ) ;
#7806 = ADVANCED_FACE ( 'NONE', ( #4994 ), #1618, .T. ) ;
#7807 = VECTOR ( 'NONE', #4871, 1000.000000000000227 ) ;
#7808 = CARTESIAN_POINT ( 'NONE',  ( 114.1489752661110089, -25.18526831983100323, 3.399999999999999911 ) ) ;
#7809 = ORIENTED_EDGE ( 'NONE', *, *, #20297, .F. ) ;
#7810 = DIRECTION ( 'NONE',  ( 3.469446951953605354E-14, 9.757819552369514663E-14, -1.000000000000000000 ) ) ;
#7811 = FACE_OUTER_BOUND ( 'NONE', #3879, .T. ) ;
#7812 = ORIENTED_EDGE ( 'NONE', *, *, #11599, .T. ) ;
#7813 = ITEM_DEFINED_TRANSFORMATION ( 'NONE', 'NONE', #20080,  #12739 ) ;
#7814 = CARTESIAN_POINT ( 'NONE',  ( -17.00058718854806017, -0.04792152746387605411, 3.750000000000000000 ) ) ;
#7815 = ORIENTED_EDGE ( 'NONE', *, *, #12647, .F. ) ;
#7816 = DATE_TIME_ROLE ( 'creation_date' ) ;
#7817 = CARTESIAN_POINT ( 'NONE',  ( -12.50000000434420144, 26.95208919326699970, -6.749999999997279510 ) ) ;
#7818 = ORIENTED_EDGE ( 'NONE', *, *, #4069, .F. ) ;
#7819 = ORIENTED_EDGE ( 'NONE', *, *, #12479, .F. ) ;
#7820 = PLANE ( 'NONE',  #2770 ) ;
#7821 = MECHANICAL_CONTEXT ( 'NONE', #1690, 'mechanical' ) ;
#7822 = VECTOR ( 'NONE', #8320, 999.9999999999998863 ) ;
#7823 = ADVANCED_FACE ( 'NONE', ( #10944 ), #3568, .F. ) ;
#7824 = SECURITY_CLASSIFICATION_LEVEL ( 'unclassified' ) ;
#7825 = DIRECTION ( 'NONE',  ( -0.2306359803922027607, -0.9730401042858035643, 0.000000000000000000 ) ) ;
#7826 = EDGE_CURVE ( 'NONE', #17755, #21398, #5678, .T. ) ;
#7827 = DIRECTION ( 'NONE',  ( 0.000000000000000000, 0.000000000000000000, 1.000000000000000000 ) ) ;
#7828 = DIRECTION ( 'NONE',  ( -1.213490492418603984E-15, -4.861311874477930828E-15, -1.000000000000000000 ) ) ;
#7829 = ORIENTED_EDGE ( 'NONE', *, *, #2846, .F. ) ;
#7830 = EDGE_CURVE ( 'NONE', #8196, #19161, #16599, .T. ) ;
#7831 = APPROVAL_ROLE ( '' ) ;
#7832 = CONICAL_SURFACE ( 'NONE', #22613, 2.283500000000000085, 0.7853981633974447263 ) ;
#7833 = ADVANCED_FACE ( 'NONE', ( #12934 ), #18168, .F. ) ;
#7834 = AXIS2_PLACEMENT_3D ( 'NONE', #13770, #4623, #11769 ) ;
#7835 = EDGE_LOOP ( 'NONE', ( #5340, #12149, #18160, #8254 ) ) ;
#7836 = CARTESIAN_POINT ( 'NONE',  ( 113.8430260960419957, 8.210644904773758412, 3.037748485030009753E-14 ) ) ;
#7837 = ORIENTED_EDGE ( 'NONE', *, *, #10647, .F. ) ;
#7838 = DIRECTION ( 'NONE',  ( -0.2306359803922026497, -0.9730401042858035643, 0.000000000000000000 ) ) ;
#7839 = DIRECTION ( 'NONE',  ( 0.2306359803922080343, 0.9730401042858022320, -3.554125915991511201E-14 ) ) ;
#7840 = DIRECTION ( 'NONE',  ( 0.9730401042858035643, -0.2306359803922027607, 0.000000000000000000 ) ) ;
#7841 = ORIENTED_EDGE ( 'NONE', *, *, #19138, .F. ) ;
#7842 = ORIENTED_EDGE ( 'NONE', *, *, #16626, .T. ) ;
#7843 = CARTESIAN_POINT ( 'NONE',  ( -20.00000000000000000, -20.00000000000000000, 0.000000000000000000 ) ) ;
#7844 = EDGE_LOOP ( 'NONE', ( #14186, #20921, #17534, #19071 ) ) ;
#7845 = COORDINATED_UNIVERSAL_TIME_OFFSET ( 0, 0, .AHEAD. ) ;
#7846 = ORIENTED_EDGE ( 'NONE', *, *, #12471, .T. ) ;
#7847 = ORIENTED_EDGE ( 'NONE', *, *, #15006, .T. ) ;
#7848 = DIRECTION ( 'NONE',  ( 0.2306359803922031215, 0.9730401042858034533, -4.741332172907939802E-18 ) ) ;
#7849 = APPROVAL_DATE_TIME ( #9654, #9994 ) ;
#7850 = CARTESIAN_POINT ( 'NONE',  ( -20.00000000397270128, 22.95208919256889857, 4.454121720691780225E-12 ) ) ;
#7851 = VECTOR ( 'NONE', #9338, 1000.000000000000000 ) ;
#7852 = DIRECTION ( 'NONE',  ( 0.2306359803922076457, 0.9730401042858023430, -1.412237191019970710E-17 ) ) ;
#7853 = AXIS2_PLACEMENT_3D ( 'NONE', #2725, #13643, #17224 ) ;
#7854 = AXIS2_PLACEMENT_3D ( 'NONE', #3815, #7405, #14637 ) ;
#7855 = PRODUCT_RELATED_PRODUCT_CATEGORY ( 'detail', '', ( #5504 ) ) ;
#7856 = CARTESIAN_POINT ( 'NONE',  ( 0.000000000000000000, 0.000000000000000000, 0.000000000000000000 ) ) ;
#7857 = DIRECTION ( 'NONE',  ( -0.9730401042858036753, 0.2306359803922028995, -2.740969466505749537E-16 ) ) ;
#7858 = CALENDAR_DATE ( 2026, 31, 10 ) ;
#7859 = ORIENTED_EDGE ( 'NONE', *, *, #2811, .T. ) ;
#7860 = AXIS2_PLACEMENT_3D ( 'NONE', #5147, #17506, #1098 ) ;
#7861 = LINE ( 'NONE', #5714, #15175 ) ;
#7862 = LINE ( 'NONE', #11220, #8230 ) ;
#7863 = ORIENTED_EDGE ( 'NONE', *, *, #14216, .T. ) ;
#7864 = AXIS2_PLACEMENT_3D ( 'NONE', #31, #7304, #3261 ) ;
#7865 = DIRECTION ( 'NONE',  ( -0.2306359803922076457, -0.9730401042858024541, 1.412237191019896446E-17 ) ) ;
#7866 = AXIS2_PLACEMENT_3D ( 'NONE', #2755, #20795, #23035 ) ;
#7867 = LINE ( 'NONE', #13333, #4652 ) ;
#7868 = EDGE_LOOP ( 'NONE', ( #18893, #8727, #7294, #18801 ) ) ;
#7869 = CARTESIAN_POINT ( 'NONE',  ( 39.37089837072279863, 22.23982225285499936, -13.00000000000049916 ) ) ;
#7870 = PERSON_AND_ORGANIZATION ( #11966, #8758 ) ;
#7871 = EDGE_CURVE ( 'NONE', #7718, #813, #5817, .T. ) ;
#7872 = ORIENTED_EDGE ( 'NONE', *, *, #7042, .F. ) ;
#7873 = ORIENTED_EDGE ( 'NONE', *, *, #1397, .T. ) ;
#7874 = FACE_OUTER_BOUND ( 'NONE', #19186, .T. ) ;
#7875 = CARTESIAN_POINT ( 'NONE',  ( 41.17437060284130013, 11.63805410277969976, 20.00000000000000000 ) ) ;
#7876 = CIRCLE ( 'NONE', #10932, 2.600000000000000089 ) ;
#7877 = EDGE_LOOP ( 'NONE', ( #20407, #11366 ) ) ;
#7878 = CALENDAR_DATE ( 2026, 31, 10 ) ;
#7879 = DIRECTION ( 'NONE',  ( -0.005235963827117002221, 0.9999862922474493931, 2.636227439667000721E-16 ) ) ;
#7880 = DIRECTION ( 'NONE',  ( -4.033639808943980242E-37, 5.936300330036069670E-19, -1.000000000000000000 ) ) ;
#7881 = VECTOR ( 'NONE', #19372, 1000.000000000000114 ) ;
#7882 = APPROVAL_DATE_TIME ( #20349, #6762 ) ;
#7883 = CARTESIAN_POINT ( 'NONE',  ( 5.000000000000000000, -27.34999999999999787, -2.500000000000000000 ) ) ;
#7884 = CIRCLE ( 'NONE', #2578, 2.500000000000000444 ) ;
#7885 = CIRCLE ( 'NONE', #14322, 3.499999999999998668 ) ;
#7886 =( NAMED_UNIT ( * ) SI_UNIT ( $, .STERADIAN. ) SOLID_ANGLE_UNIT ( ) );
#7887 = CARTESIAN_POINT ( 'NONE',  ( -26.68810977484059777, -6.639828994528159889, 2.500000000000090150 ) ) ;
#7888 = PLANE ( 'NONE',  #12819 ) ;
#7889 = PERSON_AND_ORGANIZATION ( #11966, #8758 ) ;
#7890 = FACE_OUTER_BOUND ( 'NONE', #2965, .T. ) ;
#7891 = AXIS2_PLACEMENT_3D ( 'NONE', #12682, #23102, #5088 ) ;
#7892 = CARTESIAN_POINT ( 'NONE',  ( 34.40556712239440174, 8.514986143070949254, -27.69000000000049866 ) ) ;
#7893 = FACE_OUTER_BOUND ( 'NONE', #3379, .T. ) ;
#7894 = DIRECTION ( 'NONE',  ( 1.159535895544890222E-14, 2.167612681253619929E-15, 1.000000000000000000 ) ) ;
#7895 = CIRCLE ( 'NONE', #5994, 2.499999999999998668 ) ;
#7896 = DIRECTION ( 'NONE',  ( -0.2306359803922102825, -0.9730401042858017879, 4.857225732735058287E-15 ) ) ;
#7897 = CARTESIAN_POINT ( 'NONE',  ( -12.09504422718935857, 22.14054384521797303, -3.294210050729730189E-15 ) ) ;
#7898 = ORIENTED_EDGE ( 'NONE', *, *, #22094, .F. ) ;
#7899 = EDGE_CURVE ( 'NONE', #22544, #21046, #3670, .T. ) ;
#7900 = ORIENTED_EDGE ( 'NONE', *, *, #67, .F. ) ;
#7901 = CARTESIAN_POINT ( 'NONE',  ( -32.42721070416779838, 10.33414378941739997, -5.000000000000000000 ) ) ;
#7902 = VECTOR ( 'NONE', #4305, 1000.000000000000000 ) ;
#7903 = DIRECTION ( 'NONE',  ( 0.9999862922474493931, 0.005235963827101436548, -1.466966272681988813E-16 ) ) ;
#7904 = EDGE_LOOP ( 'NONE', ( #338, #3688, #19908, #20763 ) ) ;
#7905 = CC_DESIGN_PERSON_AND_ORGANIZATION_ASSIGNMENT ( #10424, #10068, ( #1966 ) ) ;
#7906 = DIRECTION ( 'NONE',  ( -3.099353312215988811E-62, 0.000000000000000000, 1.000000000000000000 ) ) ;
#7907 = ORIENTED_EDGE ( 'NONE', *, *, #1811, .F. ) ;
#7908 = DIRECTION ( 'NONE',  ( -0.7070970883417637687, -0.003702385528188433840, 0.7071067811865477948 ) ) ;
#7909 = COORDINATED_UNIVERSAL_TIME_OFFSET ( 0, 0, .AHEAD. ) ;
#7910 = PLANE ( 'NONE',  #3667 ) ;
#7911 = APPLICATION_CONTEXT ( 'configuration controlled 3d designs of mechanical parts and assemblies' ) ;
#7912 = ADVANCED_FACE ( 'NONE', ( #9140 ), #3777, .T. ) ;
#7913 = EDGE_CURVE ( 'NONE', #18943, #2977, #16419, .T. ) ;
#7914 = PERSON_AND_ORGANIZATION_ROLE ( 'classification_officer' ) ;
#7915 = DIRECTION ( 'NONE',  ( -0.9997648976141043642, -0.02168293104402130994, 0.000000000000000000 ) ) ;
#7916 = DIRECTION ( 'NONE',  ( 4.028143194477080210E-16, 2.054129435991050111E-15, 1.000000000000000000 ) ) ;
#7917 = ORIENTED_EDGE ( 'NONE', *, *, #13142, .T. ) ;
#7918 = CIRCLE ( 'NONE', #11320, 2.380000000000002114 ) ;
#7919 = DIRECTION ( 'NONE',  ( -0.9730401042858024541, 0.2306359803922080898, 5.959266323863172718E-17 ) ) ;
#7920 = VERTEX_POINT ( 'NONE', #7713 ) ;
#7921 = DIRECTION ( 'NONE',  ( -0.9999862922474493931, -0.005235963827108420544, 0.000000000000000000 ) ) ;
#7922 = DIRECTION ( 'NONE',  ( 0.2306359803922053142, 0.9730401042858028982, 0.000000000000000000 ) ) ;
#7923 = ORIENTED_EDGE ( 'NONE', *, *, #5113, .F. ) ;
#7924 =( BOUNDED_CURVE ( )  B_SPLINE_CURVE ( 2, ( #12675, #21667, #7327 ),
 .UNSPECIFIED., .F., .F. ) 
 B_SPLINE_CURVE_WITH_KNOTS ( ( 3, 3 ),
 ( 0.000000000000000000, 0.1168436138077977582 ),
 .UNSPECIFIED. ) 
 CURVE ( )  GEOMETRIC_REPRESENTATION_ITEM ( )  RATIONAL_B_SPLINE_CURVE ( ( 1.000000000000000000, 1.077350269189633059, 1.077350269189629950 ) ) 
 REPRESENTATION_ITEM ( '' )  );
#7925 = FACE_OUTER_BOUND ( 'NONE', #11448, .T. ) ;
#7926 = DIRECTION ( 'NONE',  ( -0.9997648975362233292, -0.02168293463497999313, 0.000000000000000000 ) ) ;
#7927 = ORIENTED_EDGE ( 'NONE', *, *, #19139, .F. ) ;
#7928 = UNCERTAINTY_MEASURE_WITH_UNIT (LENGTH_MEASURE( 1.000000000000000082E-05 ), #4646, 'distance_accuracy_value', 'NONE');
#7929 = EDGE_CURVE ( 'NONE', #7095, #15424, #7338, .T. ) ;
#7930 = DATE_AND_TIME ( #6268, #21317 ) ;
#7931 = CYLINDRICAL_SURFACE ( 'NONE', #21685, 2.499999999999998668 ) ;
#7932 = ORIENTED_EDGE ( 'NONE', *, *, #14403, .F. ) ;
#7934 = SECURITY_CLASSIFICATION_LEVEL ( 'unclassified' ) ;
#7933 = APPROVAL ( #19824, 'UNSPECIFIED' ) ;
#7935 = CARTESIAN_POINT ( 'NONE',  ( -20.00000000000190070, -20.00000000000000000, -8.249999999995459632 ) ) ;
#7936 = ORIENTED_EDGE ( 'NONE', *, *, #22988, .F. ) ;
#7937 = EDGE_LOOP ( 'NONE', ( #19553, #2825, #13481, #17374, #8577, #22290 ) ) ;
#7938 = APPROVAL ( #15199, 'UNSPECIFIED' ) ;
#7939 = DIRECTION ( 'NONE',  ( 0.2306359803922080898, 0.9730401042858024541, -2.572202231434325988E-16 ) ) ;
#7940 = PERSON_AND_ORGANIZATION ( #11966, #8758 ) ;
#7941 = EDGE_CURVE ( 'NONE', #11874, #19234, #8475, .T. ) ;
#7942 = EDGE_CURVE ( 'NONE', #6041, #5830, #22095, .T. ) ;
#7943 = ADVANCED_BREP_SHAPE_REPRESENTATION ( '', ( #9215, #12739 ), #1146 ) ;
#7944 = APPROVAL ( #575, 'UNSPECIFIED' ) ;
#7945 = CONTEXT_DEPENDENT_SHAPE_REPRESENTATION ( #8872, #760 ) ;
#7946 = DIRECTION ( 'NONE',  ( 0.000000000000000000, 0.000000000000000000, 1.000000000000000000 ) ) ;
#7947 = CC_DESIGN_SECURITY_CLASSIFICATION ( #18177, ( #23484 ) ) ;
#7948 = AXIS2_PLACEMENT_3D ( 'NONE', #17011, #7999, #6089 ) ;
#7949 = CARTESIAN_POINT ( 'NONE',  ( 36.84099409957970295, 22.83947580187469839, -13.00000000000049916 ) ) ;
#7950 = ORIENTED_EDGE ( 'NONE', *, *, #21394, .T. ) ;
#7951 = CALENDAR_DATE ( 2026, 31, 10 ) ;
#7952 = ORIENTED_EDGE ( 'NONE', *, *, #21702, .F. ) ;
#7953 =( REPRESENTATION_RELATIONSHIP ('NONE','NONE', #23243, #20817 ) REPRESENTATION_RELATIONSHIP_WITH_TRANSFORMATION ( #8295 )SHAPE_REPRESENTATION_RELATIONSHIP( ) );
#7954 = LINE ( 'NONE', #22426, #12957 ) ;
#7955 = CARTESIAN_POINT ( 'NONE',  ( -19.99975861755300244, 22.95209442650120124, 4.999999999999900524 ) ) ;
#7956 = ORIENTED_EDGE ( 'NONE', *, *, #10889, .F. ) ;
#7957 = ADVANCED_FACE ( 'NONE', ( #11301 ), #16489, .F. ) ;
#7958 = PLANE ( 'NONE',  #20030 ) ;
#7959 = FACE_OUTER_BOUND ( 'NONE', #11645, .T. ) ;
#7960 = DIRECTION ( 'NONE',  ( -0.9730401042858035643, 0.2306359803922028717, 5.958148513035547083E-17 ) ) ;
#7961 = EDGE_LOOP ( 'NONE', ( #17953, #7145, #14701, #1294, #20366 ) ) ;
#7962 = SECURITY_CLASSIFICATION ( '', '', #3563 ) ;
#7963 = EDGE_LOOP ( 'NONE', ( #14229, #14785, #17793, #16406, #6957, #10111, #22202, #6350, #20456 ) ) ;
#7965 = CARTESIAN_POINT ( 'NONE',  ( 39.90784330637245603, 24.93874613768034010, 12.99999999999970512 ) ) ;
#7964 = CIRCLE ( 'NONE', #21221, 2.500000000000000000 ) ;
#7966 = ORIENTED_EDGE ( 'NONE', *, *, #22295, .T. ) ;
#7967 = APPROVAL_DATE_TIME ( #17098, #7938 ) ;
#7968 = EDGE_LOOP ( 'NONE', ( #14353, #11779, #11431, #10022 ) ) ;
#7969 = ORIENTED_EDGE ( 'NONE', *, *, #10434, .T. ) ;
#7970 = FACE_OUTER_BOUND ( 'NONE', #6247, .T. ) ;
#7971 = VECTOR ( 'NONE', #11828, 999.9999999999998863 ) ;
#7972 = PERSON_AND_ORGANIZATION ( #11966, #8758 ) ;
#7973 = EDGE_CURVE ( 'NONE', #1408, #14586, #18052, .T. ) ;
#7974 = DIRECTION ( 'NONE',  ( -6.123237831918399306E-17, 1.586917373610080078E-30, 1.000000000000000000 ) ) ;
#7975 = EDGE_CURVE ( 'NONE', #15056, #6828, #13772, .T. ) ;
#7976 = DIRECTION ( 'NONE',  ( 1.213490492418610097E-15, 4.861311874477940294E-15, 1.000000000000000000 ) ) ;
#7977 = SECURITY_CLASSIFICATION ( '', '', #10479 ) ;
#7978 = SHAPE_REPRESENTATION_RELATIONSHIP ( 'NONE' , 'NONE' ,  #22961, #18729 ) ;
#7979 = VECTOR ( 'NONE', #16675, 1000.000000000000227 ) ;
#7980 = AXIS2_PLACEMENT_3D ( 'NONE', #17450, #20892, #10002 ) ;
#7981 = CARTESIAN_POINT ( 'NONE',  ( 39.67523673029199927, 5.313293424922040487, -15.90000000000000036 ) ) ;
#7982 = COORDINATED_UNIVERSAL_TIME_OFFSET ( 0, 0, .AHEAD. ) ;
#7983 = EDGE_LOOP ( 'NONE', ( #1666, #18303, #15551, #2870, #12029, #12411, #20046, #7360 ) ) ;
#7984 = CARTESIAN_POINT ( 'NONE',  ( 83.62762864230479920, -14.97056015138829821, 13.00000000000000000 ) ) ;
#7985 = DIRECTION ( 'NONE',  ( -1.000000000000000000, 8.326672684687908612E-17, 0.000000000000000000 ) ) ;
#7986 = CIRCLE ( 'NONE', #6446, 2.066999999999999726 ) ;
#7987 = ORIENTED_EDGE ( 'NONE', *, *, #8545, .F. ) ;
#7988 = FACE_OUTER_BOUND ( 'NONE', #16969, .T. ) ;
#7989 = LINE ( 'NONE', #1070, #19434 ) ;
#7990 = CIRCLE ( 'NONE', #3047, 2.009240000000000137 ) ;
#7991 = ORIENTED_EDGE ( 'NONE', *, *, #23206, .T. ) ;
#7992 = CARTESIAN_POINT ( 'NONE',  ( -20.00000000000000000, -15.00000000000000000, -5.499999999995480060 ) ) ;
#7993 = DATE_AND_TIME ( #721, #13 ) ;
#7994 = PRODUCT_DEFINITION_SHAPE ( 'NONE', 'NONE',  #23512 ) ;
#7995 = APPROVAL_PERSON_ORGANIZATION ( #1318, #10128, #13810 ) ;
#7996 = ORIENTED_EDGE ( 'NONE', *, *, #12235, .F. ) ;
#7997 = ORIENTED_EDGE ( 'NONE', *, *, #13062, .F. ) ;
#7998 = CYLINDRICAL_SURFACE ( 'NONE', #18322, 6.500000000000000888 ) ;
#7999 = DIRECTION ( 'NONE',  ( -1.138590270679730064E-14, -2.220446049251240387E-15, -1.000000000000000000 ) ) ;
#8000 =( GEOMETRIC_REPRESENTATION_CONTEXT ( 3 ) GLOBAL_UNCERTAINTY_ASSIGNED_CONTEXT ( ( #8500 ) ) GLOBAL_UNIT_ASSIGNED_CONTEXT ( ( #6619, #19542, #15748 ) ) REPRESENTATION_CONTEXT ( 'NONE', 'WORKASPACE' ) );
#8001 = EDGE_LOOP ( 'NONE', ( #10515, #22314, #22249, #2282 ) ) ;
#8002 = PERSON_AND_ORGANIZATION ( #11966, #8758 ) ;
#8003 = CARTESIAN_POINT ( 'NONE',  ( 114.1489752661110089, -25.18526831983100323, -3.400000000000049649 ) ) ;
#8004 = CARTESIAN_POINT ( 'NONE',  ( -19.99975861755289941, 22.95209442650110176, 5.000000000000000000 ) ) ;
#8005 = SECURITY_CLASSIFICATION_LEVEL ( 'unclassified' ) ;
#8006 = DIRECTION ( 'NONE',  ( 0.2306359803922087282, 0.9730401042858021210, 2.478176394252581732E-15 ) ) ;
#8007 =( NAMED_UNIT ( * ) SI_UNIT ( $, .STERADIAN. ) SOLID_ANGLE_UNIT ( ) );
#8008 = EDGE_CURVE ( 'NONE', #587, #5237, #2120, .T. ) ;
#8009 = CARTESIAN_POINT ( 'NONE',  ( 1.133770560463819718E-13, -8.411617717272179750E-16, 8.874009851233079243E-14 ) ) ;
#8010 = APPLICATION_PROTOCOL_DEFINITION ( 'international standard', 'config_control_design', 1994, #17631 ) ;
#8011 = LOCAL_TIME ( 14, 11, 27.00000000000000000, #20642 ) ;
#8012 = APPROVAL_PERSON_ORGANIZATION ( #12949, #1247, #226 ) ;
#8013 = CARTESIAN_POINT ( 'NONE',  ( -23.49893655333865894, 22.87624079303418156, 3.749999999999949818 ) ) ;
#8014 = CARTESIAN_POINT ( 'NONE',  ( -30.15704507771850018, 9.287077397714901039, -5.000000000000000000 ) ) ;
#8016 = CARTESIAN_POINT ( 'NONE',  ( 33.90884364377009774, 10.17428291754630010, 27.68999999999999773 ) ) ;
#8015 = VECTOR ( 'NONE', #2219, 1000.000000000000227 ) ;
#8017 = DIRECTION ( 'NONE',  ( -0.9730401042858035643, 0.2306359803922028717, 5.958148513035547083E-17 ) ) ;
#8018 = SECURITY_CLASSIFICATION ( '', '', #21105 ) ;
#8019 = DIRECTION ( 'NONE',  ( -0.8648054144888007722, -0.5021071549687909918, -5.295409231245618283E-17 ) ) ;
#8020 = VECTOR ( 'NONE', #10540, 1000.000000000000000 ) ;
#8021 = VERTEX_POINT ( 'NONE', #14486 ) ;
#8022 = EDGE_LOOP ( 'NONE', ( #8263, #8434, #18506, #16046 ) ) ;
#8023 = PLANE ( 'NONE',  #3882 ) ;
#8024 = DIRECTION ( 'NONE',  ( 0.005225493764090578461, -0.9999863470142587030, 2.442038948239898212E-15 ) ) ;
#8025 = ORIENTED_EDGE ( 'NONE', *, *, #22281, .T. ) ;
#8026 = PLANE ( 'NONE',  #18711 ) ;
#8027 = ORIENTED_EDGE ( 'NONE', *, *, #4301, .T. ) ;
#8028 = LOCAL_TIME ( 14, 11, 27.00000000000000000, #19045 ) ;
#8029 = CARTESIAN_POINT ( 'NONE',  ( 35.59419854219520118, 9.774809681453278998, -21.50000000000000000 ) ) ;
#8030 = APPROVAL_PERSON_ORGANIZATION ( #14522, #16991, #6943 ) ;
#8031 = PERSON_AND_ORGANIZATION_ROLE ( 'creator' ) ;
#8032 = TOROIDAL_SURFACE ( 'NONE', #21294, 3.750000000000000000, 0.5000000000000000000 ) ;
#8033 = DIRECTION ( 'NONE',  ( -3.210834492181040124E-17, 2.441916418604790135E-15, 1.000000000000000000 ) ) ;
#8034 = DATE_TIME_ROLE ( 'classification_date' ) ;
#8035 = CC_DESIGN_APPROVAL ( #5436, ( #12599 ) ) ;
#8036 = DIRECTION ( 'NONE',  ( 3.121716675495546285E-31, 4.969341027148640384E-15, 1.000000000000000000 ) ) ;
#8037 = EDGE_CURVE ( 'NONE', #18213, #2561, #11274, .T. ) ;
#8038 = CARTESIAN_POINT ( 'NONE',  ( -24.50000000000000000, -28.60000000000000142, 21.50000000000000000 ) ) ;
#8039 = VERTEX_POINT ( 'NONE', #21720 ) ;
#8040 = DIRECTION ( 'NONE',  ( 0.000000000000000000, 1.000000000000000000, -5.551115123125781913E-15 ) ) ;
#8041 = LOCAL_TIME ( 14, 11, 27.00000000000000000, #4987 ) ;
#8042 = CARTESIAN_POINT ( 'NONE',  ( 35.59419854219520118, 9.774809681453540122, 26.30000000000000071 ) ) ;
#8043 = ORIENTED_EDGE ( 'NONE', *, *, #16314, .T. ) ;
#8044 = CARTESIAN_POINT ( 'NONE',  ( 34.60900853987882897, 7.952645293563162632, -8.774947752588866834 ) ) ;
#8045 = CIRCLE ( 'NONE', #20933, 4.999999999999995559 ) ;
#8046 = DIRECTION ( 'NONE',  ( 2.269747459789000104E-13, 2.220446049250330436E-15, 1.000000000000000000 ) ) ;
#8047 = EDGE_CURVE ( 'NONE', #7920, #23387, #5461, .T. ) ;
#8048 = ADVANCED_FACE ( 'NONE', ( #12714, #17215 ), #20762, .T. ) ;
#8049 = APPROVAL_STATUS ( 'not_yet_approved' ) ;
#8050 = AXIS2_PLACEMENT_3D ( 'NONE', #6031, #10085, #22757 ) ;
#8051 = CARTESIAN_POINT ( 'NONE',  ( -26.68810977484059777, -6.639828994528159889, 9.265539023039960360E-14 ) ) ;
#8052 = SECURITY_CLASSIFICATION ( '', '', #7575 ) ;
#8053 = ORIENTED_EDGE ( 'NONE', *, *, #5726, .F. ) ;
#8054 = DATE_TIME_ROLE ( 'classification_date' ) ;
#8055 = LINE ( 'NONE', #15291, #23200 ) ;
#8056 = ORIENTED_EDGE ( 'NONE', *, *, #15520, .T. ) ;
#8057 = ORIENTED_EDGE ( 'NONE', *, *, #22462, .T. ) ;
#8058 = CIRCLE ( 'NONE', #21321, 2.499999999999999112 ) ;
#8059 = CALENDAR_DATE ( 2026, 31, 10 ) ;
#8060 = LOCAL_TIME ( 14, 11, 27.00000000000000000, #14360 ) ;
#8061 = CALENDAR_DATE ( 2026, 31, 10 ) ;
#8062 = CARTESIAN_POINT ( 'NONE',  ( 39.67523673029199927, 5.313293424921989860, 18.89999999999999858 ) ) ;
#8063 = CIRCLE ( 'NONE', #5412, 7.999999999999997335 ) ;
#8064 = ADVANCED_FACE ( 'NONE', ( #4140 ), #857, .T. ) ;
#8065 = VECTOR ( 'NONE', #6995, 1000.000000000000000 ) ;
#8066 =( BOUNDED_CURVE ( )  B_SPLINE_CURVE ( 2, ( #4237, #18755, #4476 ),
 .UNSPECIFIED., .F., .F. ) 
 B_SPLINE_CURVE_WITH_KNOTS ( ( 3, 3 ),
 ( 0.000000000000000000, 0.1752654207116860208 ),
 .UNSPECIFIED. ) 
 CURVE ( )  GEOMETRIC_REPRESENTATION_ITEM ( )  RATIONAL_B_SPLINE_CURVE ( ( 1.000000000000000000, 1.154700538379239916, 1.000000000000000000 ) ) 
 REPRESENTATION_ITEM ( '' )  );
#8067 = CARTESIAN_POINT ( 'NONE',  ( -56.96862724498259922, -24.85214435119530307, -5.538187069399500051E-15 ) ) ;
#8068 = ORIENTED_EDGE ( 'NONE', *, *, #14162, .F. ) ;
#8069 = CC_DESIGN_PERSON_AND_ORGANIZATION_ASSIGNMENT ( #6868, #8648, ( #15652 ) ) ;
#8070 = VECTOR ( 'NONE', #21154, 1000.000000000000114 ) ;
#8071 = PERSON_AND_ORGANIZATION ( #11966, #8758 ) ;
#8072 = CC_DESIGN_PERSON_AND_ORGANIZATION_ASSIGNMENT ( #3179, #6748, ( #14088 ) ) ;
#8073 = ORIENTED_EDGE ( 'NONE', *, *, #12008, .T. ) ;
#8074 = CIRCLE ( 'NONE', #21344, 0.2000000000000016209 ) ;
#8075 = DIRECTION ( 'NONE',  ( -0.1630842657209340962, -0.6880432561069589337, -0.7071067811865457964 ) ) ;
#8076 = DIRECTION ( 'NONE',  ( 1.224646799147353207E-16, 1.000000000000000000, -0.000000000000000000 ) ) ;
#8077 = ORIENTED_EDGE ( 'NONE', *, *, #18565, .F. ) ;
#8078 = CIRCLE ( 'NONE', #16033, 0.5000000000000000000 ) ;
#8079 = EDGE_CURVE ( 'NONE', #15778, #18815, #6576, .T. ) ;
#8080 = EDGE_CURVE ( 'NONE', #8503, #7688, #797, .T. ) ;
#8081 = LOCAL_TIME ( 14, 11, 27.00000000000000000, #3870 ) ;
#8082 = CARTESIAN_POINT ( 'NONE',  ( -22.52506282043209751, 26.45208917575140006, -6.749999999994999555 ) ) ;
#8083 = ADVANCED_FACE ( 'NONE', ( #8297 ), #13637, .F. ) ;
#8084 = CYLINDRICAL_SURFACE ( 'NONE', #21012, 2.500000000000001776 ) ;
#8085 = LINE ( 'NONE', #10107, #93 ) ;
#8086 = ORIENTED_EDGE ( 'NONE', *, *, #1384, .F. ) ;
#8087 = ORIENTED_EDGE ( 'NONE', *, *, #18381, .T. ) ;
#8088 = CARTESIAN_POINT ( 'NONE',  ( 117.1933702072879981, -12.34113894325840022, -19.59999999999999787 ) ) ;
#8089 = AXIS2_PLACEMENT_3D ( 'NONE', #23012, #2613, #17579 ) ;
#8090 = VERTEX_POINT ( 'NONE', #13519 ) ;
#8091 = AXIS2_PLACEMENT_3D ( 'NONE', #14406, #8959, #5506 ) ;
#8092 = PERSON_AND_ORGANIZATION ( #11966, #8758 ) ;
#8093 = EDGE_LOOP ( 'NONE', ( #21736, #2092 ) ) ;
#8094 = CIRCLE ( 'NONE', #15279, 2.750000000000002220 ) ;
#8095 = ORIENTED_EDGE ( 'NONE', *, *, #9589, .T. ) ;
#8096 = CARTESIAN_POINT ( 'NONE',  ( 37.27955344062029752, 9.375336445360519022, -27.69000000000049866 ) ) ;
#8097 = PERSON_AND_ORGANIZATION ( #11966, #8758 ) ;
#8098 = FACE_OUTER_BOUND ( 'NONE', #8093, .T. ) ;
#8099 = VECTOR ( 'NONE', #4085, 1000.000000000000114 ) ;
#8100 = AXIS2_PLACEMENT_3D ( 'NONE', #21353, #15999, #21223 ) ;
#8101 = ADVANCED_FACE ( 'NONE', ( #22766 ), #20649, .T. ) ;
#8102 = ORGANIZATION ( 'NAUO-ORG4', 'UNSPECIFIED', 'UNSPECIFIED' ) ;
#8103 = AXIS2_PLACEMENT_3D ( 'NONE', #14318, #18364, #20129 ) ;
#8104 = AXIS2_PLACEMENT_3D ( 'NONE', #10037, #6690, #19164 ) ;
#8105 = CARTESIAN_POINT ( 'NONE',  ( 35.13079550495195491, 7.819738582318261244, 10.50000000000021139 ) ) ;
#8106 = COORDINATED_UNIVERSAL_TIME_OFFSET ( 0, 0, .AHEAD. ) ;
#8107 = AXIS2_PLACEMENT_3D ( 'NONE', #5864, #20347, #4077 ) ;
#8108 = ORIENTED_EDGE ( 'NONE', *, *, #1703, .F. ) ;
#8109 = CARTESIAN_POINT ( 'NONE',  ( -56.98461483124570037, -21.79876819407909849, -1.072991366992009803E-14 ) ) ;
#8110 = DIRECTION ( 'NONE',  ( 0.2306359803922025109, 0.9730401042858035643, -5.112869192352692394E-15 ) ) ;
#8111 = VERTEX_POINT ( 'NONE', #2600 ) ;
#8112 = EDGE_CURVE ( 'NONE', #16843, #15787, #16850, .T. ) ;
#8113 = ADVANCED_FACE ( 'NONE', ( #4494, #10095 ), #18989, .T. ) ;
#8114 = DIRECTION ( 'NONE',  ( -6.123230199561429643E-17, -4.868008300101910084E-15, -1.000000000000000000 ) ) ;
#8115 = CARTESIAN_POINT ( 'NONE',  ( -30.72441677844230057, -6.660963241697680282, 5.500000000000089706 ) ) ;
#8116 = ORIENTED_EDGE ( 'NONE', *, *, #2603, .T. ) ;
#8117 = CIRCLE ( 'NONE', #11168, 6.000000000001507239 ) ;
#8118 = CYLINDRICAL_SURFACE ( 'NONE', #7675, 2.066999999999997950 ) ;
#8119 = APPROVAL_ROLE ( '' ) ;
#8120 = AXIS2_PLACEMENT_3D ( 'NONE', #13612, #7919, #4360 ) ;
#8121 = ORIENTED_EDGE ( 'NONE', *, *, #12351, .F. ) ;
#8122 = ORIENTED_EDGE ( 'NONE', *, *, #7767, .F. ) ;
#8123 = DIRECTION ( 'NONE',  ( 1.013160721610911865E-47, -1.000000000000000000, 2.441916418604790135E-15 ) ) ;
#8124 = CARTESIAN_POINT ( 'NONE',  ( 43.84419854219520829, -33.09999999999999432, -21.50000000000000000 ) ) ;
#8125 = ORIENTED_EDGE ( 'NONE', *, *, #13319, .F. ) ;
#8126 = VECTOR ( 'NONE', #4034, 999.9999999999998863 ) ;
#8127 = COORDINATED_UNIVERSAL_TIME_OFFSET ( 0, 0, .AHEAD. ) ;
#8128 = LINE ( 'NONE', #8003, #10770 ) ;
#8129 = CARTESIAN_POINT ( 'NONE',  ( -23.49917714535047963, 22.87619892134707200, -3.750000000000059508 ) ) ;
#8130 = APPROVAL_STATUS ( 'not_yet_approved' ) ;
#8131 = LINE ( 'NONE', #15117, #4061 ) ;
#8132 = ADVANCED_FACE ( 'NONE', ( #2836 ), #1031, .T. ) ;
#8133 = CYLINDRICAL_SURFACE ( 'NONE', #18909, 2.500000000000000444 ) ;
#8134 = APPROVAL_DATE_TIME ( #2655, #18024 ) ;
#8135 = AXIS2_PLACEMENT_3D ( 'NONE', #13476, #11483, #9693 ) ;
#8136 = ADVANCED_FACE ( 'NONE', ( #11541 ), #18775, .T. ) ;
#8137 = PLANE ( 'NONE',  #18760 ) ;
#8138 = AXIS2_PLACEMENT_3D ( 'NONE', #5206, #17445, #6656 ) ;
#8139 = CARTESIAN_POINT ( 'NONE',  ( 58.73439644601030096, 17.65016624305009785, -13.00000000000049916 ) ) ;
#8140 = EDGE_CURVE ( 'NONE', #16195, #4635, #101, .T. ) ;
#8141 = DIRECTION ( 'NONE',  ( -6.662161100567945949E-09, 1.000000000000000000, -2.081668171172169697E-15 ) ) ;
#8142 = DIRECTION ( 'NONE',  ( -0.9730401042858035643, 0.2306359803922028717, 5.958148513035547083E-17 ) ) ;
#8143 = CARTESIAN_POINT ( 'NONE',  ( 34.24699604337060066, 12.59578995394270073, 3.750000000000000000 ) ) ;
#8144 = DIRECTION ( 'NONE',  ( -0.9730401042858036753, 0.2306359803922024831, 0.000000000000000000 ) ) ;
#8145 = ORIENTED_EDGE ( 'NONE', *, *, #2694, .T. ) ;
#8146 = EDGE_LOOP ( 'NONE', ( #611, #21373, #4111 ) ) ;
#8147 = DIRECTION ( 'NONE',  ( 0.9730401042858024541, -0.2306359803922080898, -5.959266323858952312E-17 ) ) ;
#8148 = DIRECTION ( 'NONE',  ( 1.000000000000000000, -6.124317834331790129E-17, 0.000000000000000000 ) ) ;
#8149 = VERTEX_POINT ( 'NONE', #15067 ) ;
#8150 = CARTESIAN_POINT ( 'NONE',  ( 35.89100945995100034, 24.25134070964839950, -15.00000000000049916 ) ) ;
#8151 = ORIENTED_EDGE ( 'NONE', *, *, #4356, .T. ) ;
#8152 = DIRECTION ( 'NONE',  ( -0.9730401042858023430, 0.2306359803922080620, 5.959266323858944916E-17 ) ) ;
#8153 = CALENDAR_DATE ( 2026, 31, 10 ) ;
#8154 = LINE ( 'NONE', #17293, #5200 ) ;
#8155 = DIRECTION ( 'NONE',  ( 0.9730401042858035643, -0.2306359803922028717, -5.959266323858677443E-17 ) ) ;
#8156 = APPROVAL ( #21973, 'UNSPECIFIED' ) ;
#8157 = CARTESIAN_POINT ( 'NONE',  ( -61.39998491075132847, -25.32193520680032961, 4.999999999999990230 ) ) ;
#8158 = DIRECTION ( 'NONE',  ( 0.9730401042858036753, -0.2306359803922028995, -5.958148513035547083E-17 ) ) ;
#8159 = ORIENTED_EDGE ( 'NONE', *, *, #6819, .T. ) ;
#8160 = DIRECTION ( 'NONE',  ( -0.2306359803922033436, -0.9730401042858034533, 0.000000000000000000 ) ) ;
#8161 = AXIS2_PLACEMENT_3D ( 'NONE', #15529, #19456, #10455 ) ;
#8162 = CARTESIAN_POINT ( 'NONE',  ( 3.499952022866071211, 0.01832587339492581721, 8.822666031689207903E-14 ) ) ;
#8163 = ORIENTED_EDGE ( 'NONE', *, *, #1354, .F. ) ;
#8164 = PLANE ( 'NONE',  #8617 ) ;
#8165 = DIRECTION ( 'NONE',  ( 0.005235963827104182615, -0.9999862922474495042, -7.400535959113083303E-19 ) ) ;
#8166 = CALENDAR_DATE ( 2026, 31, 10 ) ;
#8167 = LINE ( 'NONE', #18762, #23260 ) ;
#8168 = VERTEX_POINT ( 'NONE', #8067 ) ;
#8169 = ORIENTED_EDGE ( 'NONE', *, *, #19869, .F. ) ;
#8170 = DATE_AND_TIME ( #21211, #5371 ) ;
#8171 = CARTESIAN_POINT ( 'NONE',  ( -22.49941224781415627, 22.89788185598131420, -3.750000000000000000 ) ) ;
#8172 = ADVANCED_FACE ( 'NONE', ( #2484 ), #922, .T. ) ;
#8173 = ORIENTED_EDGE ( 'NONE', *, *, #18283, .T. ) ;
#8174 = VERTEX_POINT ( 'NONE', #22649 ) ;
#8175 = DIRECTION ( 'NONE',  ( -0.2306359803922028440, -0.9730401042858034533, -4.307366329831518561E-32 ) ) ;
#8176 = APPLICATION_PROTOCOL_DEFINITION ( 'international standard', 'config_control_design', 1994, #22956 ) ;
#8177 = AXIS2_PLACEMENT_3D ( 'NONE', #5304, #12567, #21919 ) ;
#8178 = APPROVAL_STATUS ( 'not_yet_approved' ) ;
#8179 = CARTESIAN_POINT ( 'NONE',  ( 43.40226860240920814, 19.16001186014064572, 13.00000000000000000 ) ) ;
#8180 = EDGE_CURVE ( 'NONE', #4592, #6410, #22300, .T. ) ;
#8181 = EDGE_CURVE ( 'NONE', #9514, #2018, #12286, .T. ) ;
#8182 = CARTESIAN_POINT ( 'NONE',  ( -20.00019857044559757, 22.95165872133759777, -3.750000000000059508 ) ) ;
#8183 = ORIENTED_EDGE ( 'NONE', *, *, #19222, .F. ) ;
#8184 = PERSON_AND_ORGANIZATION ( #11966, #8758 ) ;
#8185 = PRODUCT ( '1602p_c_13', '1602p_c_13', '', ( #6896 ) ) ;
#8186 = VERTEX_POINT ( 'NONE', #13416 ) ;
#8187 = DIRECTION ( 'NONE',  ( -0.7194962871189621856, -0.6944962871189651610, -2.229973200609260484E-62 ) ) ;
#8188 = LINE ( 'NONE', #6399, #16947 ) ;
#8189 = ORIENTED_EDGE ( 'NONE', *, *, #9317, .F. ) ;
#8190 = FACE_OUTER_BOUND ( 'NONE', #17157, .T. ) ;
#8191 = CARTESIAN_POINT ( 'NONE',  ( -20.00000000397270128, 22.95208919257349933, 6.750000000004470202 ) ) ;
#8192 = DIRECTION ( 'NONE',  ( -2.982858504577324546E-17, 2.441916418604795262E-15, 1.000000000000000000 ) ) ;
#8193 = ORIENTED_EDGE ( 'NONE', *, *, #9525, .F. ) ;
#8194 = ORIENTED_EDGE ( 'NONE', *, *, #7093, .F. ) ;
#8195 = CARTESIAN_POINT ( 'NONE',  ( 38.22140682376686982, 9.152092534394576262, 26.30000000000000426 ) ) ;
#8196 = VERTEX_POINT ( 'NONE', #15659 ) ;
#8197 = DATE_AND_TIME ( #17237, #20900 ) ;
#8198 = VECTOR ( 'NONE', #3732, 1000.000000000000000 ) ;
#8199 = EDGE_CURVE ( 'NONE', #17821, #19182, #11953, .T. ) ;
#8200 = VERTEX_POINT ( 'NONE', #10457 ) ;
#8201 = ORIENTED_EDGE ( 'NONE', *, *, #21811, .F. ) ;
#8202 = CARTESIAN_POINT ( 'NONE',  ( -20.00000000000000000, -20.00000000000000000, 5.000000000000000000 ) ) ;
#8203 = COORDINATED_UNIVERSAL_TIME_OFFSET ( 0, 0, .AHEAD. ) ;
#8204 = CC_DESIGN_PERSON_AND_ORGANIZATION_ASSIGNMENT ( #6580, #13692, ( #6423 ) ) ;
#8205 = CC_DESIGN_PERSON_AND_ORGANIZATION_ASSIGNMENT ( #8346, #15583, ( #16907 ) ) ;
#8206 = DIRECTION ( 'NONE',  ( -0.8823529412199652144, 0.4705882352125652091, 9.020562075079389002E-15 ) ) ;
#8207 =( BOUNDED_CURVE ( )  B_SPLINE_CURVE ( 2, ( #3063, #19219, #10333 ),
 .UNSPECIFIED., .F., .F. ) 
 B_SPLINE_CURVE_WITH_KNOTS ( ( 3, 3 ),
 ( 0.000000000000000000, 0.2336872276155859962 ),
 .UNSPECIFIED. ) 
 CURVE ( )  GEOMETRIC_REPRESENTATION_ITEM ( )  RATIONAL_B_SPLINE_CURVE ( ( 1.000000000000000000, 1.154700538379259900, 1.000000000000000000 ) ) 
 REPRESENTATION_ITEM ( '' )  );
#8208 = EDGE_CURVE ( 'NONE', #14326, #2641, #8078, .T. ) ;
#8209 = EDGE_CURVE ( 'NONE', #14761, #15790, #14897, .T. ) ;
#8210 = AXIS2_PLACEMENT_3D ( 'NONE', #7570, #5545, #12802 ) ;
#8211 = CARTESIAN_POINT ( 'NONE',  ( 0.000000000000000000, -17.30000000000000071, -5.000000000000000000 ) ) ;
#8212 = COORDINATED_UNIVERSAL_TIME_OFFSET ( 0, 0, .AHEAD. ) ;
#8213 = ORIENTED_EDGE ( 'NONE', *, *, #18380, .T. ) ;
#8214 = CYLINDRICAL_SURFACE ( 'NONE', #2295, 2.500000000000000000 ) ;
#8215 = LINE ( 'NONE', #19258, #12800 ) ;
#8216 = VERTEX_POINT ( 'NONE', #17905 ) ;
#8217 = DIRECTION ( 'NONE',  ( 0.000000000000000000, 0.000000000000000000, -1.000000000000000000 ) ) ;
#8218 = CARTESIAN_POINT ( 'NONE',  ( 31.01827548281339375, -2.500766059351137827, -11.00000000000039435 ) ) ;
#8219 = ORIENTED_EDGE ( 'NONE', *, *, #20431, .F. ) ;
#8220 = DIRECTION ( 'NONE',  ( 0.000000000000000000, 0.000000000000000000, -1.000000000000000000 ) ) ;
#8221 = APPLICATION_CONTEXT ( 'configuration controlled 3d designs of mechanical parts and assemblies' ) ;
#8222 = PERSON_AND_ORGANIZATION ( #11966, #8758 ) ;
#8223 = ADVANCED_FACE ( 'NONE', ( #17685 ), #8654, .T. ) ;
#8224 = AXIS2_PLACEMENT_3D ( 'NONE', #4120, #18757, #17056 ) ;
#8225 = ORIENTED_EDGE ( 'NONE', *, *, #18352, .T. ) ;
#8226 = ORIENTED_EDGE ( 'NONE', *, *, #3541, .T. ) ;
#8227 = CARTESIAN_POINT ( 'NONE',  ( 35.35837847849400362, 22.00420084508159846, 11.00000000000000000 ) ) ;
#8228 = AXIS2_PLACEMENT_3D ( 'NONE', #13359, #2187, #8141 ) ;
#8229 = PLANE ( 'NONE',  #21377 ) ;
#8230 = VECTOR ( 'NONE', #16999, 1000.000000000000227 ) ;
#8231 = EDGE_LOOP ( 'NONE', ( #1266, #20040, #6376, #5156 ) ) ;
#8232 = APPROVAL_DATE_TIME ( #18819, #2542 ) ;
#8233 = PLANE ( 'NONE',  #8107 ) ;
#8234 = CC_DESIGN_PERSON_AND_ORGANIZATION_ASSIGNMENT ( #15059, #8540, ( #13292 ) ) ;
#8235 = PRODUCT_RELATED_PRODUCT_CATEGORY ( 'detail', '', ( #1883 ) ) ;
#8236 = CARTESIAN_POINT ( 'NONE',  ( 33.91130781617516732, -0.3602965737506598209, -12.99999999999999645 ) ) ;
#8237 = DATE_AND_TIME ( #13470, #15145 ) ;
#8238 = DIRECTION ( 'NONE',  ( 0.000000000000000000, 0.000000000000000000, 1.000000000000000000 ) ) ;
#8239 = EDGE_CURVE ( 'NONE', #8907, #16864, #17201, .T. ) ;
#8240 = EDGE_CURVE ( 'NONE', #563, #2422, #14161, .T. ) ;
#8241 = PERSON ( 'NAUO-PER4', 'UNSPECIFIED', 'UNSPECIFIED', ('UNSPECIFIED'), ('UNSPECIFIED'), ('UNSPECIFIED') ) ;
#8242 =( NAMED_UNIT ( * ) SI_UNIT ( $, .STERADIAN. ) SOLID_ANGLE_UNIT ( ) );
#8243 = CARTESIAN_POINT ( 'NONE',  ( 39.27359436029389883, 22.26288585089424998, -13.00000000000030020 ) ) ;
#8244 = DATE_TIME_ROLE ( 'creation_date' ) ;
#8245 = CONICAL_SURFACE ( 'NONE', #7864, 2.693275000000006081, 0.7853166638051269910 ) ;
#8246 = CONICAL_SURFACE ( 'NONE', #2564, 0.8660254037844395958, 1.047197551196598297 ) ;
#8247 = CARTESIAN_POINT ( 'NONE',  ( -19.99999998648642574, 20.32708919256890212, -8.249999999995543121 ) ) ;
#8248 = DIRECTION ( 'NONE',  ( 0.9730401042858035643, -0.2306359803922028717, 2.740969466505749044E-16 ) ) ;
#8249 = DIRECTION ( 'NONE',  ( 0.000000000000000000, 0.000000000000000000, 1.000000000000000000 ) ) ;
#8250 = CARTESIAN_POINT ( 'NONE',  ( 30.76933207471821774, -4.221800468112557603, -12.00000000000039968 ) ) ;
#8251 = AXIS2_PLACEMENT_3D ( 'NONE', #5512, #12761, #7880 ) ;
#8252 = CARTESIAN_POINT ( 'NONE',  ( 5.750000000000129674, -20.33108891324529921, 2.500000000000000000 ) ) ;
#8253 = CARTESIAN_POINT ( 'NONE',  ( -20.00000000397270128, 22.95208919256889857, -4.999999999995559996 ) ) ;
#8254 = ORIENTED_EDGE ( 'NONE', *, *, #6935, .T. ) ;
#8255 = EDGE_CURVE ( 'NONE', #12003, #13977, #3914, .T. ) ;
#8256 = ORIENTED_EDGE ( 'NONE', *, *, #5924, .T. ) ;
#8257 = LINE ( 'NONE', #12313, #8834 ) ;
#8258 = CARTESIAN_POINT ( 'NONE',  ( -16.50000000000000000, -20.00000000000000000, -5.000000000000000000 ) ) ;
#8259 = VECTOR ( 'NONE', #4888, 1000.000000000000000 ) ;
#8260 = ORIENTED_EDGE ( 'NONE', *, *, #8903, .T. ) ;
#8261 = DIRECTION ( 'NONE',  ( -3.099353312215988811E-62, 0.000000000000000000, 1.000000000000000000 ) ) ;
#8262 = AXIS2_PLACEMENT_3D ( 'NONE', #1251, #21086, #15509 ) ;
#8263 = ORIENTED_EDGE ( 'NONE', *, *, #1412, .T. ) ;
#8264 = CIRCLE ( 'NONE', #20760, 2.600000000000000089 ) ;
#8265 = DIRECTION ( 'NONE',  ( 0.2306359803922094498, 0.9730401042858018990, 0.000000000000000000 ) ) ;
#8266 = CIRCLE ( 'NONE', #13577, 2.600000000000000089 ) ;
#8267 = PERSON_AND_ORGANIZATION ( #11966, #8758 ) ;
#8268 = DIRECTION ( 'NONE',  ( 0.9730401042858024541, -0.2306359803922080898, -5.959266323858942451E-17 ) ) ;
#8269 = EDGE_CURVE ( 'NONE', #21354, #20926, #10211, .T. ) ;
#8270 = EDGE_CURVE ( 'NONE', #16036, #14838, #6760, .T. ) ;
#8271 = SECURITY_CLASSIFICATION_LEVEL ( 'unclassified' ) ;
#8272 = AXIS2_PLACEMENT_3D ( 'NONE', #17676, #11877, #11993 ) ;
#8273 = CARTESIAN_POINT ( 'NONE',  ( -20.00000000000000000, -20.00000000000000000, 2.500000000000000000 ) ) ;
#8274 = CARTESIAN_POINT ( 'NONE',  ( -14.00000000397399980, 22.95208919312840123, -5.499999999996930455 ) ) ;
#8275 = DIRECTION ( 'NONE',  ( 1.000000000000000000, 0.000000000000000000, 0.000000000000000000 ) ) ;
#8276 = DIRECTION ( 'NONE',  ( -6.662112528310618598E-09, 1.000000000000000000, -2.081668171172169697E-15 ) ) ;
#8277 = ORIENTED_EDGE ( 'NONE', *, *, #1696, .F. ) ;
#8278 = CARTESIAN_POINT ( 'NONE',  ( -62.91413607658799378, 7.983193290926554830, -2.458499999999998131 ) ) ;
#8279 = AXIS2_PLACEMENT_3D ( 'NONE', #20254, #3973, #16795 ) ;
#8280 = LINE ( 'NONE', #6374, #17097 ) ;
#8281 = AXIS2_PLACEMENT_3D ( 'NONE', #484, #18797, #9771 ) ;
#8282 = ORIENTED_EDGE ( 'NONE', *, *, #2407, .F. ) ;
#8283 = CARTESIAN_POINT ( 'NONE',  ( 34.49266682421115604, 8.020563254273458398, -8.783920975641599682 ) ) ;
#8284 = DIRECTION ( 'NONE',  ( 6.123230174520370177E-17, 4.962644601432260272E-15, 1.000000000000000000 ) ) ;
#8285 = CONTEXT_DEPENDENT_SHAPE_REPRESENTATION ( #19776, #2487 ) ;
#8286 = CARTESIAN_POINT ( 'NONE',  ( 31.49315201223960159, -2.613324229818040134, 13.00000000000019895 ) ) ;
#8287 = VERTEX_POINT ( 'NONE', #16120 ) ;
#8288 = ORIENTED_EDGE ( 'NONE', *, *, #4384, .T. ) ;
#8289 = CC_DESIGN_PERSON_AND_ORGANIZATION_ASSIGNMENT ( #8324, #12028, ( #1510 ) ) ;
#8290 = APPROVAL_STATUS ( 'not_yet_approved' ) ;
#8291 = FACE_OUTER_BOUND ( 'NONE', #21994, .T. ) ;
#8292 = ORIENTED_EDGE ( 'NONE', *, *, #12034, .T. ) ;
#8293 = CARTESIAN_POINT ( 'NONE',  ( -23.49917714535047963, 22.87619892134707200, -2.500000000000059952 ) ) ;
#8294 = MECHANICAL_CONTEXT ( 'NONE', #20803, 'mechanical' ) ;
#8295 = ITEM_DEFINED_TRANSFORMATION ( 'NONE', 'NONE', #13649,  #12739 ) ;
#8296 = CARTESIAN_POINT ( 'NONE',  ( 88.98991518642354492, 7.652622273256637797, 12.99999999999970157 ) ) ;
#8297 = FACE_OUTER_BOUND ( 'NONE', #12044, .T. ) ;
#8298 = ORIENTED_EDGE ( 'NONE', *, *, #12555, .F. ) ;
#8299 = ADVANCED_FACE ( 'NONE', ( #13988 ), #8765, .T. ) ;
#8300 = PERSON_AND_ORGANIZATION_ROLE ( 'creator' ) ;
#8301 = VERTEX_POINT ( 'NONE', #8418 ) ;
#8302 = DIRECTION ( 'NONE',  ( 0.000000000000000000, 0.000000000000000000, 1.000000000000000000 ) ) ;
#8303 = CARTESIAN_POINT ( 'NONE',  ( -26.68881687192900287, -6.639832696913689603, -2.500292893218899692 ) ) ;
#8304 = VERTEX_POINT ( 'NONE', #4732 ) ;
#8305 = FACE_OUTER_BOUND ( 'NONE', #12603, .T. ) ;
#8306 = CLOSED_SHELL ( 'NONE', ( #3570, #4973, #6810, #16778, #16191, #3707, #20742, #17439, #14046, #23340, #3853, #6758, #21050, #8172, #2897, #23461, #11715 ) ) ;
#8307 = CARTESIAN_POINT ( 'NONE',  ( 44.09191575480141978, 23.94701142199374289, -13.00000000000029665 ) ) ;
#8308 = CARTESIAN_POINT ( 'NONE',  ( -20.00000000397469790, 22.95208919256889857, -8.499999999995548450 ) ) ;
#8309 = ORIENTED_EDGE ( 'NONE', *, *, #3107, .T. ) ;
#8310 = ORIENTED_EDGE ( 'NONE', *, *, #14344, .F. ) ;
#8311 = CARTESIAN_POINT ( 'NONE',  ( 36.07092311366587722, 11.78608357701199694, -37.44562646538080486 ) ) ;
#8312 = ORIENTED_EDGE ( 'NONE', *, *, #10326, .F. ) ;
#8313 = PERSON_AND_ORGANIZATION_ROLE ( 'creator' ) ;
#8314 = ORIENTED_EDGE ( 'NONE', *, *, #17807, .T. ) ;
#8315 = ORIENTED_EDGE ( 'NONE', *, *, #15468, .T. ) ;
#8316 = CARTESIAN_POINT ( 'NONE',  ( 31.01827548281339375, -2.500766059351137827, -11.00000000000039435 ) ) ;
#8317 = B_SPLINE_CURVE_WITH_KNOTS ( 'NONE', 3,
 ( #9228, #12900, #11376, #18490, #7674, #13378, #9713, #14919, #16926, #22151, #2088, #5892, #13141, #18610, #4355, #7794, #2325, #9588, #22261, #16818, #18252, #1968, #16458, #176, #7444, #21915, #11150, #5649 ),
 .UNSPECIFIED., .F., .F.,
 ( 4, 2, 2, 2, 2, 2, 2, 2, 2, 2, 2, 2, 2, 4 ),
 ( 0.000000000000000000, 0.0004072576943254699561, 0.0008145153886509399121, 0.001629030777301882426, 0.002036288471627355906, 0.002443546165952829169, 0.002850803860278303299, 0.003258061554603776128, 0.004072576943254728292, 0.004479834637580206759, 0.004887092331905683491, 0.005294350026231164560, 0.005701607720556645630, 0.006516123109207627717 ),
 .UNSPECIFIED. ) ;
#8318 = PERSON_AND_ORGANIZATION_ROLE ( 'design_supplier' ) ;
#8319 = VECTOR ( 'NONE', #5047, 1000.000000000000000 ) ;
#8320 = DIRECTION ( 'NONE',  ( 0.9730401042858036753, -0.2306359803922028995, -5.958148513035547083E-17 ) ) ;
#8321 = CARTESIAN_POINT ( 'NONE',  ( 35.11747397072455357, 7.763535785894623231, -8.759424124906624698 ) ) ;
#8322 = CARTESIAN_POINT ( 'NONE',  ( 46.93847685464109531, -4.150000499290836586, 13.00000000000000000 ) ) ;
#8323 = EDGE_CURVE ( 'NONE', #19758, #8816, #5093, .T. ) ;
#8324 = PERSON_AND_ORGANIZATION ( #11966, #8758 ) ;
#8325 = PRODUCT ( '1602p_c_23', '1602p_c_23', '', ( #15290 ) ) ;
#8326 = ORIENTED_EDGE ( 'NONE', *, *, #17806, .T. ) ;
#8327 = LOCAL_TIME ( 14, 11, 27.00000000000000000, #2118 ) ;
#8328 = CARTESIAN_POINT ( 'NONE',  ( 31.37708959083939675, -0.2124270449897310287, 13.00000000000019895 ) ) ;
#8329 = AXIS2_PLACEMENT_3D ( 'NONE', #22472, #18575, #725 ) ;
#8330 = CARTESIAN_POINT ( 'NONE',  ( -30.79177721110609767, 6.338862259904598950, 2.999707106781179800 ) ) ;
#8331 = ORIENTED_EDGE ( 'NONE', *, *, #12868, .T. ) ;
#8332 = CC_DESIGN_PERSON_AND_ORGANIZATION_ASSIGNMENT ( #3060, #8762, ( #9926 ) ) ;
#8333 = DIRECTION ( 'NONE',  ( -0.9999862922474491711, -0.005235963827128305680, 1.734723475976808327E-16 ) ) ;
#8334 = DIRECTION ( 'NONE',  ( 0.9730401042858024541, -0.2306359803922080898, -5.959266323859172946E-17 ) ) ;
#8335 = DIRECTION ( 'NONE',  ( 0.005235963827110212514, -0.9999862922474493931, -5.936218956700083401E-19 ) ) ;
#8336 = VERTEX_POINT ( 'NONE', #12353 ) ;
#8337 = LINE ( 'NONE', #15574, #2363 ) ;
#8338 = EDGE_CURVE ( 'NONE', #14253, #9773, #1389, .T. ) ;
#8339 = ADVANCED_FACE ( 'NONE', ( #7004 ), #19460, .F. ) ;
#8340 = APPLICATION_PROTOCOL_DEFINITION ( 'international standard', 'config_control_design', 1994, #924 ) ;
#8341 = ORIENTED_EDGE ( 'NONE', *, *, #310, .T. ) ;
#8342 = VERTEX_POINT ( 'NONE', #5197 ) ;
#8343 = DIRECTION ( 'NONE',  ( -2.269700743865584947E-13, -2.220446049247695246E-15, -1.000000000000000000 ) ) ;
#8344 = CARTESIAN_POINT ( 'NONE',  ( -65.82123935389580538, 11.86253283145240012, 5.000000000000000000 ) ) ;
#8345 = EDGE_LOOP ( 'NONE', ( #10845, #10610 ) ) ;
#8346 = PERSON_AND_ORGANIZATION ( #11966, #8758 ) ;
#8347 = DIRECTION ( 'NONE',  ( 0.2306359803922053142, 0.9730401042858028982, 0.000000000000000000 ) ) ;
#8348 = DIRECTION ( 'NONE',  ( -0.9997651245102161521, -0.02167246670483386276, 0.000000000000000000 ) ) ;
#8349 = AXIS2_PLACEMENT_3D ( 'NONE', #18847, #4570, #8510 ) ;
#8350 = ITEM_DEFINED_TRANSFORMATION ( 'NONE', 'NONE', #11417,  #12739 ) ;
#8351 = AXIS2_PLACEMENT_3D ( 'NONE', #699, #11315, #7602 ) ;
#8352 = DIRECTION ( 'NONE',  ( -0.9730401042858024541, 0.2306359803922080898, 5.959266323858942451E-17 ) ) ;
#8353 =( NAMED_UNIT ( * ) PLANE_ANGLE_UNIT ( ) SI_UNIT ( $, .RADIAN. ) );
#8354 = AXIS2_PLACEMENT_3D ( 'NONE', #4684, #13937, #21061 ) ;
#8355 = DIRECTION ( 'NONE',  ( -0.9997651245102240347, -0.02167246670447264822, 0.000000000000000000 ) ) ;
#8356 = EDGE_CURVE ( 'NONE', #16192, #20851, #22887, .T. ) ;
#8357 = SHAPE_DEFINITION_REPRESENTATION ( #9105, #18121 ) ;
#8358 = CARTESIAN_POINT ( 'NONE',  ( 36.57773002789497241, 11.59782464082818798, 8.774845639077975434 ) ) ;
#8359 = CARTESIAN_POINT ( 'NONE',  ( 2.664535259100379799E-14, 6.659954201878760116E-16, 2.500000000000000000 ) ) ;
#8360 = CC_DESIGN_PERSON_AND_ORGANIZATION_ASSIGNMENT ( #22890, #10559, ( #15652 ) ) ;
#8361 = DIRECTION ( 'NONE',  ( 0.000000000000000000, -1.000000000000000000, 0.000000000000000000 ) ) ;
#8362 = LOCAL_TIME ( 14, 11, 27.00000000000000000, #10127 ) ;
#8363 = DIRECTION ( 'NONE',  ( 0.005235963827117002221, -0.9999862922474493931, -2.636227439667000721E-16 ) ) ;
#8364 = CC_DESIGN_PERSON_AND_ORGANIZATION_ASSIGNMENT ( #13057, #18632, ( #7624 ) ) ;
#8365 = DIRECTION ( 'NONE',  ( 0.000000000000000000, -1.000000000000000000, 1.534091707905539548E-92 ) ) ;
#8366 = EDGE_LOOP ( 'NONE', ( #21497, #17406, #9181, #10061 ) ) ;
#8367 = DIRECTION ( 'NONE',  ( 0.000000000000000000, -0.9999588795606766389, 0.009068582455715226351 ) ) ;
#8368 = EDGE_CURVE ( 'NONE', #3079, #13595, #22897, .T. ) ;
#8369 = AXIS2_PLACEMENT_3D ( 'NONE', #15374, #9814, #17032 ) ;
#8371 = EDGE_LOOP ( 'NONE', ( #10114, #4497, #15023, #7607, #21225 ) ) ;
#8370 = EDGE_CURVE ( 'NONE', #22329, #17785, #8207, .T. ) ;
#8372 = CC_DESIGN_PERSON_AND_ORGANIZATION_ASSIGNMENT ( #13639, #15308, ( #20866 ) ) ;
#8373 = ORIENTED_EDGE ( 'NONE', *, *, #369, .T. ) ;
#8374 = CARTESIAN_POINT ( 'NONE',  ( 39.83668191656649782, 5.994421497922140851, 18.89999999999999858 ) ) ;
#8375 = CARTESIAN_POINT ( 'NONE',  ( -19.88588018851017125, 25.44948316784238074, 5.500000000004452438 ) ) ;
#8376 = ORIENTED_EDGE ( 'NONE', *, *, #3571, .F. ) ;
#8377 = VECTOR ( 'NONE', #9033, 1000.000000000000227 ) ;
#8378 = DIRECTION ( 'NONE',  ( 2.676216343273230621E-30, -3.491853980617010126E-15, 1.000000000000000000 ) ) ;
#8379 = VERTEX_POINT ( 'NONE', #17567 ) ;
#8380 = LINE ( 'NONE', #21188, #3404 ) ;
#8381 = COORDINATED_UNIVERSAL_TIME_OFFSET ( 0, 0, .AHEAD. ) ;
#8382 = CARTESIAN_POINT ( 'NONE',  ( 41.24356139695900225, 11.92996613406540085, 18.89999999999999858 ) ) ;
#8383 = PRODUCT_DEFINITION_FORMATION_WITH_SPECIFIED_SOURCE ( 'ANY', '', #15730, .NOT_KNOWN. ) ;
#8384 = PRODUCT_DEFINITION_FORMATION_WITH_SPECIFIED_SOURCE ( 'ANY', '', #3013, .NOT_KNOWN. ) ;
#8385 = CARTESIAN_POINT ( 'NONE',  ( 35.59419854219520118, 9.774809681453278998, -27.19000000000049866 ) ) ;
#8386 = CONICAL_SURFACE ( 'NONE', #19757, 1.154700538379250796, 1.047197551196598297 ) ;
#8387 = CARTESIAN_POINT ( 'NONE',  ( 33.87671241911665021, -0.5062525893939895383, 13.00000000000019895 ) ) ;
#8388 = EDGE_CURVE ( 'NONE', #9241, #21232, #11546, .T. ) ;
#8389 = CARTESIAN_POINT ( 'NONE',  ( 0.000000000000000000, 0.000000000000000000, 0.000000000000000000 ) ) ;
#8390 = APPROVAL_PERSON_ORGANIZATION ( #4597, #921, #20859 ) ;
#8391 = DIRECTION ( 'NONE',  ( 2.269747459788990007E-13, 2.220446049250330436E-15, 1.000000000000000000 ) ) ;
#8392 = EDGE_LOOP ( 'NONE', ( #3458, #119, #13932, #8778, #9760 ) ) ;
#8394 = AXIS2_PLACEMENT_3D ( 'NONE', #5071, #10437, #5174 ) ;
#8393 = DIRECTION ( 'NONE',  ( 0.9999862922474493931, 0.005235963827108368503, 0.000000000000000000 ) ) ;
#8395 = DIRECTION ( 'NONE',  ( 0.000000000000000000, 1.000000000000000000, 0.000000000000000000 ) ) ;
#8396 = VERTEX_POINT ( 'NONE', #12568 ) ;
#8397 = CARTESIAN_POINT ( 'NONE',  ( 33.98781586735240268, 8.467099387652083919, -8.849098278953663410 ) ) ;
#8398 = DIRECTION ( 'NONE',  ( 1.000000000000000000, -1.138590270679730064E-14, 4.484155085839414876E-45 ) ) ;
#8399 = EDGE_CURVE ( 'NONE', #11037, #4401, #14802, .T. ) ;
#8400 = PRODUCT_DEFINITION_FORMATION_WITH_SPECIFIED_SOURCE ( 'ANY', '', #21217, .NOT_KNOWN. ) ;
#8401 = ITEM_DEFINED_TRANSFORMATION ( 'NONE', 'NONE', #9486,  #12739 ) ;
#8402 = ADVANCED_FACE ( 'NONE', ( #5541 ), #5307, .T. ) ;
#8403 = CARTESIAN_POINT ( 'NONE',  ( -16.50000000000000000, -20.00000000000000000, -5.000000000000000000 ) ) ;
#8404 = CC_DESIGN_APPROVAL ( #8156, ( #19756 ) ) ;
#8405 = ORIENTED_EDGE ( 'NONE', *, *, #1369, .F. ) ;
#8406 = ORIENTED_EDGE ( 'NONE', *, *, #4516, .T. ) ;
#8407 = COORDINATED_UNIVERSAL_TIME_OFFSET ( 0, 0, .AHEAD. ) ;
#8408 = DIRECTION ( 'NONE',  ( -0.005235963827108352890, 0.9999862922474493931, 5.936218956694023463E-19 ) ) ;
#8409 = ORIENTED_EDGE ( 'NONE', *, *, #5274, .T. ) ;
#8410 = CARTESIAN_POINT ( 'NONE',  ( 118.5079952955230027, -6.794810348829390279, 15.90000000000000036 ) ) ;
#8411 = LOCAL_TIME ( 14, 11, 27.00000000000000000, #13283 ) ;
#8412 = APPLICATION_CONTEXT ( 'configuration controlled 3d designs of mechanical parts and assemblies' ) ;
#8413 = CALENDAR_DATE ( 2026, 31, 10 ) ;
#8414 = COORDINATED_UNIVERSAL_TIME_OFFSET ( 0, 0, .AHEAD. ) ;
#8415 = SHAPE_REPRESENTATION ( 'Pin 3', ( #12739 ), #3033 ) ;
#8416 = FACE_BOUND ( 'NONE', #3580, .T. ) ;
#8417 = CC_DESIGN_APPROVAL ( #7357, ( #6898 ) ) ;
#8418 = CARTESIAN_POINT ( 'NONE',  ( -24.50000000000000000, -31.09999999999999787, 21.50000000000000000 ) ) ;
#8419 = VECTOR ( 'NONE', #1394, 1000.000000000000000 ) ;
#8420 = EDGE_LOOP ( 'NONE', ( #10086, #254, #14976, #1377, #20733 ) ) ;
#8421 = VERTEX_POINT ( 'NONE', #21681 ) ;
#8422 = EDGE_CURVE ( 'NONE', #8342, #22529, #16436, .T. ) ;
#8423 = ORGANIZATION ( 'NAUO-ORG27', 'UNSPECIFIED', 'UNSPECIFIED' ) ;
#8424 = LINE ( 'NONE', #4737, #1194 ) ;
#8425 = CARTESIAN_POINT ( 'NONE',  ( 4.267766952966369765, -30.47499999999999787, -20.76776695296636888 ) ) ;
#8426 = VERTEX_POINT ( 'NONE', #1979 ) ;
#8427 = EDGE_CURVE ( 'NONE', #1644, #16863, #1270, .T. ) ;
#8428 = DIRECTION ( 'NONE',  ( 0.000000000000000000, 0.000000000000000000, -1.000000000000000000 ) ) ;
#8429 = CARTESIAN_POINT ( 'NONE',  ( -22.50000000000000000, -20.00000000000000000, -7.748383280539974188E-62 ) ) ;
#8430 = DIRECTION ( 'NONE',  ( 2.982858504489129897E-17, -2.441916418604790135E-15, -1.000000000000000000 ) ) ;
#8431 = VERTEX_POINT ( 'NONE', #7344 ) ;
#8432 = VERTEX_POINT ( 'NONE', #7450 ) ;
#8433 = DIRECTION ( 'NONE',  ( 1.000000000000000000, 0.000000000000000000, 0.000000000000000000 ) ) ;
#8434 = ORIENTED_EDGE ( 'NONE', *, *, #6230, .T. ) ;
#8435 = DATE_AND_TIME ( #21370, #9916 ) ;
#8436 = CC_DESIGN_APPROVAL ( #21859, ( #11856 ) ) ;
#8437 = EDGE_LOOP ( 'NONE', ( #16364, #16954, #9782, #3337 ) ) ;
#8438 = ORIENTED_EDGE ( 'NONE', *, *, #8768, .T. ) ;
#8439 = DIRECTION ( 'NONE',  ( 0.000000000000000000, 1.734723475976806848E-16, 1.000000000000000000 ) ) ;
#8440 = CALENDAR_DATE ( 2026, 31, 10 ) ;
#8441 = CIRCLE ( 'NONE', #4258, 2.066999999999999726 ) ;
#8442 = AXIS2_PLACEMENT_3D ( 'NONE', #6380, #17197, #18972 ) ;
#8443 = AXIS2_PLACEMENT_3D ( 'NONE', #8935, #19859, #22172 ) ;
#8444 = CARTESIAN_POINT ( 'NONE',  ( 34.74128820227589642, 24.82052816820960217, 14.50000000000000000 ) ) ;
#8445 = AXIS2_PLACEMENT_3D ( 'NONE', #13973, #12434, #19666 ) ;
#8446 = ORGANIZATION ( 'NAUO-ORG30', 'UNSPECIFIED', 'UNSPECIFIED' ) ;
#8447 = VECTOR ( 'NONE', #19755, 1000.000000000000000 ) ;
#8448 = CARTESIAN_POINT ( 'NONE',  ( 0.000000000000000000, 0.000000000000000000, 0.000000000000000000 ) ) ;
#8449 = LINE ( 'NONE', #19710, #2785 ) ;
#8450 = DIRECTION ( 'NONE',  ( -0.9730401042858024541, 0.2306359803922080898, 5.959266323858942451E-17 ) ) ;
#8451 = PERSON_AND_ORGANIZATION_ROLE ( 'classification_officer' ) ;
#8452 = SECURITY_CLASSIFICATION ( '', '', #5111 ) ;
#8453 = ORIENTED_EDGE ( 'NONE', *, *, #5053, .F. ) ;
#8454 = DIRECTION ( 'NONE',  ( 1.138590270679728013E-14, 2.220446049251240387E-15, 1.000000000000000000 ) ) ;
#8455 = CIRCLE ( 'NONE', #837, 6.499999999999998224 ) ;
#8456 = DIRECTION ( 'NONE',  ( 6.123230174520380038E-17, 4.962644601432250805E-15, 1.000000000000000000 ) ) ;
#8457 = ORIENTED_EDGE ( 'NONE', *, *, #6489, .F. ) ;
#8458 = AXIS2_PLACEMENT_3D ( 'NONE', #16555, #23454, #283 ) ;
#8459 = CARTESIAN_POINT ( 'NONE',  ( 31.01827548281339375, -2.500766059351008153, 15.00000000000011546 ) ) ;
#8460 = AXIS2_PLACEMENT_3D ( 'NONE', #17405, #12077, #10174 ) ;
#8461 = DIRECTION ( 'NONE',  ( 0.7806762821592939661, -0.6249356306644248127, -7.632783294297949638E-15 ) ) ;
#8462 = CARTESIAN_POINT ( 'NONE',  ( 120.3930287342899987, 3.035456073538489896, 13.00000000000000000 ) ) ;
#8463 = ORIENTED_EDGE ( 'NONE', *, *, #644, .F. ) ;
#8464 = CARTESIAN_POINT ( 'NONE',  ( 37.46113131852679601, -4.027891576221660053, 13.00000000000000000 ) ) ;
#8465 = CIRCLE ( 'NONE', #9986, 2.500000000000000000 ) ;
#8466 = DATE_TIME_ROLE ( 'classification_date' ) ;
#8467 = ORIENTED_EDGE ( 'NONE', *, *, #20854, .F. ) ;
#8468 = VERTEX_POINT ( 'NONE', #14685 ) ;
#8469 = DIRECTION ( 'NONE',  ( 0.9730401042858035643, -0.2306359803922029272, 1.531342102931249911E-15 ) ) ;
#8470 = DIRECTION ( 'NONE',  ( 0.000000000000000000, 0.000000000000000000, 1.000000000000000000 ) ) ;
#8471 = AXIS2_PLACEMENT_3D ( 'NONE', #21193, #13728, #20971 ) ;
#8472 = DIRECTION ( 'NONE',  ( 0.000000000000000000, 0.000000000000000000, 1.000000000000000000 ) ) ;
#8473 = COORDINATED_UNIVERSAL_TIME_OFFSET ( 0, 0, .AHEAD. ) ;
#8474 = EDGE_CURVE ( 'NONE', #17116, #3741, #15309, .T. ) ;
#8475 = CIRCLE ( 'NONE', #16796, 2.066999999999998394 ) ;
#8476 = DIRECTION ( 'NONE',  ( -0.6880432561069586006, 0.1630842657209346236, 0.7071067811865459074 ) ) ;
#8477 = EDGE_CURVE ( 'NONE', #23363, #14815, #23464, .T. ) ;
#8478 = APPROVAL_PERSON_ORGANIZATION ( #5536, #947, #12791 ) ;
#8479 = LINE ( 'NONE', #22943, #22765 ) ;
#8480 = AXIS2_PLACEMENT_3D ( 'NONE', #17446, #3075, #934 ) ;
#8481 = DIRECTION ( 'NONE',  ( 3.099353312215989243E-62, -1.534091707905539548E-92, -1.000000000000000000 ) ) ;
#8482 = VECTOR ( 'NONE', #8343, 1000.000000000000000 ) ;
#8483 = AXIS2_PLACEMENT_3D ( 'NONE', #10264, #19276, #2994 ) ;
#8484 =( LENGTH_UNIT ( ) NAMED_UNIT ( * ) SI_UNIT ( .MILLI., .METRE. ) );
#8485 = ADVANCED_FACE ( 'NONE', ( #69 ), #11164, .T. ) ;
#8486 = EDGE_CURVE ( 'NONE', #3143, #12984, #6593, .T. ) ;
#8487 = CARTESIAN_POINT ( 'NONE',  ( -19.99975861755300244, 22.95209442650120124, 2.499999999999900524 ) ) ;
#8488 = PERSON_AND_ORGANIZATION_ROLE ( 'creator' ) ;
#8489 = DIRECTION ( 'NONE',  ( 0.005235964011411631258, -0.9999862922464843873, 2.602085213965210642E-15 ) ) ;
#8490 = AXIS2_PLACEMENT_3D ( 'NONE', #16205, #23436, #7189 ) ;
#8491 = DIRECTION ( 'NONE',  ( 4.539762594625140272E-47, 1.000000000000000000, 0.000000000000000000 ) ) ;
#8492 = DIRECTION ( 'NONE',  ( 0.9730401042858035643, -0.2306359803922028717, -5.959266323858674978E-17 ) ) ;
#8493 = LOCAL_TIME ( 14, 11, 27.00000000000000000, #6968 ) ;
#8494 = VECTOR ( 'NONE', #6132, 1000.000000000000000 ) ;
#8495 = CARTESIAN_POINT ( 'NONE',  ( 30.31182762792540331, -4.706706774123539994, -13.00000000000039968 ) ) ;
#8496 = DIRECTION ( 'NONE',  ( 0.7806762821592939661, -0.6249356306644247017, -1.759009604640482141E-13 ) ) ;
#8497 = ORIENTED_EDGE ( 'NONE', *, *, #10067, .F. ) ;
#8498 = VECTOR ( 'NONE', #1953, 1000.000000000000000 ) ;
#8499 = DIRECTION ( 'NONE',  ( 0.1153179901961009640, 0.4865200521429018377, 0.8660254037844385966 ) ) ;
#8500 = UNCERTAINTY_MEASURE_WITH_UNIT (LENGTH_MEASURE( 1.000000000000000082E-05 ), #6619, 'distance_accuracy_value', 'NONE');
#8501 = VERTEX_POINT ( 'NONE', #18029 ) ;
#8502 = CIRCLE ( 'NONE', #13427, 2.066999999999997062 ) ;
#8503 = VERTEX_POINT ( 'NONE', #16569 ) ;
#8504 = CARTESIAN_POINT ( 'NONE',  ( 35.59419854219520118, 9.774809681453239918, -37.44562646538079775 ) ) ;
#8505 = DIRECTION ( 'NONE',  ( -0.9730401042858024541, 0.2306359803922080898, 5.959266323858942451E-17 ) ) ;
#8506 = ORIENTED_EDGE ( 'NONE', *, *, #9767, .F. ) ;
#8507 = FACE_OUTER_BOUND ( 'NONE', #13148, .T. ) ;
#8508 = EDGE_CURVE ( 'NONE', #11146, #17831, #9344, .T. ) ;
#8509 = ORIENTED_EDGE ( 'NONE', *, *, #19974, .F. ) ;
#8510 = DIRECTION ( 'NONE',  ( 0.000000000000000000, 0.000000000000000000, -1.000000000000000000 ) ) ;
#8511 = CALENDAR_DATE ( 2026, 31, 10 ) ;
#8512 = CARTESIAN_POINT ( 'NONE',  ( -17.54011269262000283, -27.34999999999999787, -5.000000000000000000 ) ) ;
#8513 = APPROVAL ( #17385, 'UNKNOWN' ) ;
#8514 = VECTOR ( 'NONE', #13123, 1000.000000000000000 ) ;
#8515 = CC_DESIGN_PERSON_AND_ORGANIZATION_ASSIGNMENT ( #8097, #20438, ( #10349 ) ) ;
#8516 =( LENGTH_UNIT ( ) NAMED_UNIT ( * ) SI_UNIT ( .MILLI., .METRE. ) );
#8517 = AXIS2_PLACEMENT_3D ( 'NONE', #6404, #13530, #22433 ) ;
#8518 =( REPRESENTATION_RELATIONSHIP ('NONE','NONE', #6895, #17646 ) REPRESENTATION_RELATIONSHIP_WITH_TRANSFORMATION ( #17776 )SHAPE_REPRESENTATION_RELATIONSHIP( ) );
#8519 = CARTESIAN_POINT ( 'NONE',  ( -31.64684134471649912, 7.334398819369059908, -2.500000000000000000 ) ) ;
#8520 = EDGE_CURVE ( 'NONE', #1171, #5066, #1853, .T. ) ;
#8521 = ADVANCED_FACE ( 'NONE', ( #5783 ), #502, .T. ) ;
#8522 = DIRECTION ( 'NONE',  ( -0.6944962871189651610, 0.7194962871189621856, -2.152489367803870976E-62 ) ) ;
#8523 = DIRECTION ( 'NONE',  ( 1.138590270679730064E-14, 2.220446049251245514E-15, 1.000000000000000000 ) ) ;
#8524 = ORIENTED_EDGE ( 'NONE', *, *, #10576, .T. ) ;
#8525 = CYLINDRICAL_SURFACE ( 'NONE', #14705, 2.499999999999998668 ) ;
#8526 = DESIGN_CONTEXT ( 'detailed design', #19327, 'design' ) ;
#8527 = DIRECTION ( 'NONE',  ( -0.9730401042858036753, 0.2306359803922028995, 5.958148513035547083E-17 ) ) ;
#8528 = VERTEX_POINT ( 'NONE', #18261 ) ;
#8529 = CARTESIAN_POINT ( 'NONE',  ( -27.39120887301850260, 6.327965799971420502, 3.750000000000000000 ) ) ;
#8530 = CARTESIAN_POINT ( 'NONE',  ( 31.49315201223960159, -2.613324229818040134, 13.00000000000019895 ) ) ;
#8531 = ORIENTED_EDGE ( 'NONE', *, *, #11880, .F. ) ;
#8532 = APPROVAL_STATUS ( 'not_yet_approved' ) ;
#8533 = ORIENTED_EDGE ( 'NONE', *, *, #16743, .T. ) ;
#8534 = ORIENTED_EDGE ( 'NONE', *, *, #5758, .T. ) ;
#8535 = PERSON_AND_ORGANIZATION ( #11966, #8758 ) ;
#8536 = FACE_OUTER_BOUND ( 'NONE', #16776, .T. ) ;
#8537 = EDGE_CURVE ( 'NONE', #4472, #1408, #18498, .T. ) ;
#8538 = VERTEX_POINT ( 'NONE', #21570 ) ;
#8539 = CARTESIAN_POINT ( 'NONE',  ( 38.79430841974239286, 19.80722199214058676, 13.00000000000000000 ) ) ;
#8540 = PERSON_AND_ORGANIZATION_ROLE ( 'design_owner' ) ;
#8541 = PRODUCT_DEFINITION_SHAPE ( 'NONE', 'NONE',  #4882 ) ;
#8542 = CALENDAR_DATE ( 2026, 31, 10 ) ;
#8543 = CARTESIAN_POINT ( 'NONE',  ( -22.52506283708709844, 28.95208917575130414, -5.499999999995009325 ) ) ;
#8544 = EDGE_CURVE ( 'NONE', #1934, #17514, #9465, .T. ) ;
#8545 = EDGE_CURVE ( 'NONE', #238, #19010, #7110, .T. ) ;
#8546 = CARTESIAN_POINT ( 'NONE',  ( 5.026060663935580067E-16, -1.434026569662460006E-15, 2.500000000000090150 ) ) ;
#8547 = VERTEX_POINT ( 'NONE', #7223 ) ;
#8548 = AXIS2_PLACEMENT_3D ( 'NONE', #20867, #19451, #8175 ) ;
#8549 = ORIENTED_EDGE ( 'NONE', *, *, #8338, .T. ) ;
#8550 = DIRECTION ( 'NONE',  ( 1.466984912809909902E-16, 2.805478249466310097E-20, 1.000000000000000000 ) ) ;
#8551 = CARTESIAN_POINT ( 'NONE',  ( -65.80336369117380002, 8.448563927732790191, 5.000000000000000000 ) ) ;
#8552 = ORIENTED_EDGE ( 'NONE', *, *, #2577, .F. ) ;
#8553 = DIRECTION ( 'NONE',  ( 1.138590270679734009E-14, 2.220446049251240387E-15, 1.000000000000000000 ) ) ;
#8554 = CARTESIAN_POINT ( 'NONE',  ( 45.98502771169970060, -8.172548290408343519, -13.00000000000000000 ) ) ;
#8555 = CARTESIAN_POINT ( 'NONE',  ( -19.49999999982360066, -0.1021026942259639914, 2.500000000000000000 ) ) ;
#8556 = VERTEX_POINT ( 'NONE', #10920 ) ;
#8557 = ORIENTED_EDGE ( 'NONE', *, *, #1441, .F. ) ;
#8558 = DIRECTION ( 'NONE',  ( 0.000000000000000000, 1.000000000000000000, -5.551115123125781913E-15 ) ) ;
#8559 = ORIENTED_EDGE ( 'NONE', *, *, #14630, .T. ) ;
#8560 = PERSON_AND_ORGANIZATION_ROLE ( 'classification_officer' ) ;
#8561 = ADVANCED_FACE ( 'NONE', ( #18145, #16347 ), #22386, .T. ) ;
#8562 = ORIENTED_EDGE ( 'NONE', *, *, #4909, .F. ) ;
#8563 = AXIS2_PLACEMENT_3D ( 'NONE', #920, #1387, #1027 ) ;
#8564 = VERTEX_POINT ( 'NONE', #11853 ) ;
#8565 = CARTESIAN_POINT ( 'NONE',  ( 52.93501234483859719, 21.14904221214005631, 13.00000000000000000 ) ) ;
#8566 =( BOUNDED_CURVE ( )  B_SPLINE_CURVE ( 2, ( #8616, #14197, #15854 ),
 .UNSPECIFIED., .F., .F. ) 
 B_SPLINE_CURVE_WITH_KNOTS ( ( 3, 3 ),
 ( 0.08763271035584378754, 0.1752654207116860208 ),
 .UNSPECIFIED. ) 
 CURVE ( )  GEOMETRIC_REPRESENTATION_ITEM ( )  RATIONAL_B_SPLINE_CURVE ( ( 1.077350269189625065, 1.077350269189624399, 1.000000000000000000 ) ) 
 REPRESENTATION_ITEM ( '' )  );
#8567 = APPROVAL_DATE_TIME ( #13898, #15623 ) ;
#8568 = EDGE_CURVE ( 'NONE', #13613, #14838, #22270, .T. ) ;
#8569 = DIRECTION ( 'NONE',  ( 0.9730401042858035643, -0.2306359803922028717, -5.959266323858674978E-17 ) ) ;
#8570 = EDGE_CURVE ( 'NONE', #13864, #184, #2573, .T. ) ;
#8571 = EDGE_CURVE ( 'NONE', #13133, #1632, #4114, .T. ) ;
#8572 = DIRECTION ( 'NONE',  ( 0.000000000000000000, 0.000000000000000000, -1.000000000000000000 ) ) ;
#8573 = SHAPE_DEFINITION_REPRESENTATION ( #17637, #22194 ) ;
#8574 = ORIENTED_EDGE ( 'NONE', *, *, #17400, .F. ) ;
#8575 = CARTESIAN_POINT ( 'NONE',  ( -22.50000000000000000, -20.00000001665527805, 8.000000000004588330 ) ) ;
#8576 = CARTESIAN_POINT ( 'NONE',  ( 39.67523673029199927, 5.313293424922060026, -18.89999999999999858 ) ) ;
#8577 = ORIENTED_EDGE ( 'NONE', *, *, #14434, .T. ) ;
#8578 = CONICAL_SURFACE ( 'NONE', #21074, 2.283499999999998753, 0.7853981633974433940 ) ;
#8579 = CARTESIAN_POINT ( 'NONE',  ( 27.73073027566760018, -1.721531772300955110, 13.00000000000000000 ) ) ;
#8580 = FACE_OUTER_BOUND ( 'NONE', #22104, .T. ) ;
#8581 = CARTESIAN_POINT ( 'NONE',  ( 27.03882233449100170, -4.640652085158330387, 20.00000000000000000 ) ) ;
#8582 = ORIENTED_EDGE ( 'NONE', *, *, #15181, .F. ) ;
#8583 = DIRECTION ( 'NONE',  ( -0.005235963827121952255, 0.9999862922474493931, -2.738476122049126182E-14 ) ) ;
#8584 = PERSON_AND_ORGANIZATION_ROLE ( 'creator' ) ;
#8585 = ORIENTED_EDGE ( 'NONE', *, *, #8683, .T. ) ;
#8586 = VERTEX_POINT ( 'NONE', #22157 ) ;
#8587 = CARTESIAN_POINT ( 'NONE',  ( -65.62876257020761273, -24.89748912807110059, 5.000000000000000000 ) ) ;
#8588 = DIRECTION ( 'NONE',  ( 0.9730401042858024541, -0.2306359803922080898, -5.959266323858711956E-17 ) ) ;
#8589 = COORDINATED_UNIVERSAL_TIME_OFFSET ( 0, 0, .AHEAD. ) ;
#8590 = CC_DESIGN_DATE_AND_TIME_ASSIGNMENT ( #389, #272, ( #4231 ) ) ;
#8591 = CARTESIAN_POINT ( 'NONE',  ( -55.82882037092586813, -8.292431354569982815, 7.200000000000000178 ) ) ;
#8592 = CARTESIAN_POINT ( 'NONE',  ( 39.27359436029389883, 22.26288585089439920, 12.99999999999979927 ) ) ;
#8593 = PLANE ( 'NONE',  #5882 ) ;
#8594 = CIRCLE ( 'NONE', #13517, 3.499999999999998668 ) ;
#8595 = DIRECTION ( 'NONE',  ( 0.000000000000000000, 0.000000000000000000, 1.000000000000000000 ) ) ;
#8596 = DIRECTION ( 'NONE',  ( -0.2306359803922033158, -0.9730401042858034533, 0.000000000000000000 ) ) ;
#8597 = COORDINATED_UNIVERSAL_TIME_OFFSET ( 0, 0, .AHEAD. ) ;
#8598 = DIRECTION ( 'NONE',  ( 2.269747459789000104E-13, 2.220446049250330436E-15, 1.000000000000000000 ) ) ;
#8599 = LINE ( 'NONE', #6705, #6372 ) ;
#8600 = DIRECTION ( 'NONE',  ( 1.751019220569994795E-16, 2.300154215587015208E-15, 1.000000000000000000 ) ) ;
#8601 = EDGE_CURVE ( 'NONE', #16298, #6737, #766, .T. ) ;
#8602 = AXIS2_PLACEMENT_3D ( 'NONE', #16057, #19864, #14268 ) ;
#8603 = DIRECTION ( 'NONE',  ( 0.9730401042858035643, -0.2306359803922028717, -5.959266323858677443E-17 ) ) ;
#8604 = CIRCLE ( 'NONE', #5188, 2.650000000000001688 ) ;
#8605 = FACE_BOUND ( 'NONE', #460, .T. ) ;
#8606 = EDGE_LOOP ( 'NONE', ( #14122, #11978, #17660, #4065 ) ) ;
#8607 = DIRECTION ( 'NONE',  ( 8.964882009398751025E-18, -1.954868129030600086E-15, -1.000000000000000000 ) ) ;
#8608 = VERTEX_POINT ( 'NONE', #18855 ) ;
#8609 = CARTESIAN_POINT ( 'NONE',  ( -20.00000000397270128, 22.95208919257159863, 5.500000000004459544 ) ) ;
#8610 = CARTESIAN_POINT ( 'NONE',  ( -23.50000000000000000, -20.00000000000000000, 5.000000000000000000 ) ) ;
#8611 = EDGE_LOOP ( 'NONE', ( #6283, #23232, #5689, #15895 ) ) ;
#8612 = CARTESIAN_POINT ( 'NONE',  ( -17.47493720815390006, 28.95208920939580111, -7.999999999996148858 ) ) ;
#8613 = ORIENTED_EDGE ( 'NONE', *, *, #4840, .F. ) ;
#8614 = DIRECTION ( 'NONE',  ( -0.005235963827108352890, 0.9999862922474493931, 5.936218956694023463E-19 ) ) ;
#8615 = APPLICATION_PROTOCOL_DEFINITION ( 'international standard', 'config_control_design', 1994, #22640 ) ;
#8616 = CARTESIAN_POINT ( 'NONE',  ( 35.24824457160688240, 8.315249525024842825, 27.55602540378454535 ) ) ;
#8617 = AXIS2_PLACEMENT_3D ( 'NONE', #18623, #16694, #425 ) ;
#8618 = APPROVAL_STATUS ( 'not_yet_approved' ) ;
#8619 = AXIS2_PLACEMENT_3D ( 'NONE', #11221, #8076, #3948 ) ;
#8620 = VECTOR ( 'NONE', #13828, 1000.000000000000000 ) ;
#8621 = CARTESIAN_POINT ( 'NONE',  ( 33.27705887009690144, -3.036156860537075453, 8.750000000000198952 ) ) ;
#8622 = CARTESIAN_POINT ( 'NONE',  ( -30.75845054331819739, -0.1610523420890130064, -2.999000000000079602 ) ) ;
#8623 = CARTESIAN_POINT ( 'NONE',  ( 0.000000000000000000, 0.000000000000000000, 0.000000000000000000 ) ) ;
#8624 = AXIS2_PLACEMENT_3D ( 'NONE', #14194, #21431, #5157 ) ;
#8625 = DIRECTION ( 'NONE',  ( -0.9999863470142589250, -0.005225493764064552404, 0.000000000000000000 ) ) ;
#8626 = EDGE_LOOP ( 'NONE', ( #3932, #20876, #19346, #15081 ) ) ;
#8627 = DIRECTION ( 'NONE',  ( -1.000000000000000000, -3.593595090780715053E-30, -6.123237832262829536E-17 ) ) ;
#8628 = EDGE_CURVE ( 'NONE', #7581, #20636, #22115, .T. ) ;
#8629 = CARTESIAN_POINT ( 'NONE',  ( 35.01760859121467462, 7.342209420738964987, 10.99076000000021125 ) ) ;
#8630 = VERTEX_POINT ( 'NONE', #2814 ) ;
#8631 = AXIS2_PLACEMENT_3D ( 'NONE', #1220, #15484, #22711 ) ;
#8632 = CARTESIAN_POINT ( 'NONE',  ( -65.64475015647069256, -21.84411297095480009, -5.000000000000000000 ) ) ;
#8633 = CARTESIAN_POINT ( 'NONE',  ( 0.03403376487640639991, -6.499910899608420500, 2.500000000000090150 ) ) ;
#8634 = CC_DESIGN_DATE_AND_TIME_ASSIGNMENT ( #7930, #15516, ( #22778 ) ) ;
#8635 = EDGE_LOOP ( 'NONE', ( #8077, #17509, #8983, #13895, #13787, #2198 ) ) ;
#8636 = CIRCLE ( 'NONE', #14359, 2.500000000000000000 ) ;
#8637 = DATE_AND_TIME ( #1370, #20148 ) ;
#8638 = CARTESIAN_POINT ( 'NONE',  ( -11.00000000000000000, -27.34999999999999787, -6.250000000000000000 ) ) ;
#8639 = AXIS2_PLACEMENT_3D ( 'NONE', #19843, #1423, #3673 ) ;
#8640 = ORIENTED_EDGE ( 'NONE', *, *, #17978, .F. ) ;
#8641 = VERTEX_POINT ( 'NONE', #8038 ) ;
#8642 = ADVANCED_FACE ( 'NONE', ( #899 ), #5902, .T. ) ;
#8643 = EDGE_CURVE ( 'NONE', #10115, #10197, #9597, .T. ) ;
#8644 = PERSON_AND_ORGANIZATION ( #11966, #8758 ) ;
#8645 = DIRECTION ( 'NONE',  ( 0.000000000000000000, 0.000000000000000000, -1.000000000000000000 ) ) ;
#8646 = ORIENTED_EDGE ( 'NONE', *, *, #1682, .T. ) ;
#8647 = DIRECTION ( 'NONE',  ( 0.9730401042858036753, -0.2306359803922031493, 2.804983810440361760E-16 ) ) ;
#8648 = PERSON_AND_ORGANIZATION_ROLE ( 'design_supplier' ) ;
#8649 = DATE_AND_TIME ( #19216, #23168 ) ;
#8650 = CONICAL_SURFACE ( 'NONE', #21901, 2.254620000000000068, 0.7853981633974461696 ) ;
#8651 = DIRECTION ( 'NONE',  ( 2.269747459788990007E-13, 2.220446049250330436E-15, 1.000000000000000000 ) ) ;
#8652 = CONICAL_SURFACE ( 'NONE', #21905, 1.033499999999999863, 1.029744258676650093 ) ;
#8653 = CIRCLE ( 'NONE', #12457, 3.499999999999999556 ) ;
#8654 = PLANE ( 'NONE',  #2015 ) ;
#8655 = ORIENTED_EDGE ( 'NONE', *, *, #10530, .F. ) ;
#8656 = EDGE_CURVE ( 'NONE', #17119, #5730, #12302, .T. ) ;
#8657 = ORIENTED_EDGE ( 'NONE', *, *, #20098, .F. ) ;
#8658 = CARTESIAN_POINT ( 'NONE',  ( 49.97703550743810297, 19.72589006658010291, 13.00000000000000000 ) ) ;
#8659 = DIRECTION ( 'NONE',  ( 1.099672473571039977E-13, 0.000000000000000000, -1.000000000000000000 ) ) ;
#8660 = ORIENTED_EDGE ( 'NONE', *, *, #6355, .F. ) ;
#8661 = APPROVAL ( #9739, 'UNSPECIFIED' ) ;
#8662 = CC_DESIGN_DATE_AND_TIME_ASSIGNMENT ( #5130, #4775, ( #22291 ) ) ;
#8663 = DIRECTION ( 'NONE',  ( 0.005235963827108352890, -0.9999862922474493931, -2.671135040551771006E-18 ) ) ;
#8664 = CARTESIAN_POINT ( 'NONE',  ( 43.98050001724070057, -5.573152644851429471, -15.50000000000040146 ) ) ;
#8665 = AXIS2_PLACEMENT_3D ( 'NONE', #18853, #7916, #9949 ) ;
#8666 = ORIENTED_EDGE ( 'NONE', *, *, #9214, .F. ) ;
#8667 = ORIENTED_EDGE ( 'NONE', *, *, #14601, .T. ) ;
#8668 = LINE ( 'NONE', #403, #21571 ) ;
#8669 = ORIENTED_EDGE ( 'NONE', *, *, #16798, .T. ) ;
#8670 = EDGE_CURVE ( 'NONE', #12811, #17009, #7717, .T. ) ;
#8671 = EDGE_CURVE ( 'NONE', #19719, #12125, #18752, .T. ) ;
#8672 = APPROVAL_STATUS ( 'not_yet_approved' ) ;
#8673 = ORIENTED_EDGE ( 'NONE', *, *, #5564, .F. ) ;
#8674 = ORIENTED_EDGE ( 'NONE', *, *, #15758, .F. ) ;
#8675 = APPROVAL ( #22690, 'UNSPECIFIED' ) ;
#8676 = DIRECTION ( 'NONE',  ( -3.210834492180730126E-17, 2.441916418604790135E-15, 1.000000000000000000 ) ) ;
#8677 = VECTOR ( 'NONE', #18194, 1000.000000000000000 ) ;
#8678 = CALENDAR_DATE ( 2026, 31, 10 ) ;
#8679 = DIRECTION ( 'NONE',  ( 0.000000000000000000, -1.000000000000000000, 2.081668171172168119E-15 ) ) ;
#8680 = APPLICATION_CONTEXT ( 'configuration controlled 3d designs of mechanical parts and assemblies' ) ;
#8681 = FACE_BOUND ( 'NONE', #22556, .T. ) ;
#8682 = CALENDAR_DATE ( 2026, 31, 10 ) ;
#8683 = EDGE_CURVE ( 'NONE', #6563, #17008, #17597, .T. ) ;
#8684 = CIRCLE ( 'NONE', #23072, 2.500000000000000444 ) ;
#8685 = VERTEX_POINT ( 'NONE', #6369 ) ;
#8686 = DIRECTION ( 'NONE',  ( 0.000000000000000000, -2.891431443143872083E-16, 1.000000000000000000 ) ) ;
#8687 = SPHERICAL_SURFACE ( 'NONE', #2160, 15.25000000000000000 ) ;
#8688 = ORIENTED_EDGE ( 'NONE', *, *, #5145, .F. ) ;
#8689 = EDGE_CURVE ( 'NONE', #11172, #20160, #9720, .T. ) ;
#8690 = DIRECTION ( 'NONE',  ( -0.2306359803922026497, -0.9730401042858035643, 0.000000000000000000 ) ) ;
#8691 = FACE_BOUND ( 'NONE', #14294, .T. ) ;
#8692 =( BOUNDED_CURVE ( )  B_SPLINE_CURVE ( 2, ( #23239, #7003, #1736 ),
 .UNSPECIFIED., .F., .F. ) 
 B_SPLINE_CURVE_WITH_KNOTS ( ( 3, 3 ),
 ( 0.2928548593876180162, 0.5857097187752370315 ),
 .UNSPECIFIED. ) 
 CURVE ( )  GEOMETRIC_REPRESENTATION_ITEM ( )  RATIONAL_B_SPLINE_CURVE ( ( 1.000000000000000000, 1.037954849302019866, 1.000000000000000000 ) ) 
 REPRESENTATION_ITEM ( '' )  );
#8693 = CYLINDRICAL_SURFACE ( 'NONE', #9981, 2.650000000000001688 ) ;
#8694 = ORIENTED_EDGE ( 'NONE', *, *, #21421, .F. ) ;
#8695 = CARTESIAN_POINT ( 'NONE',  ( 36.07092311366588433, 11.78608357701207865, -19.56700000000001083 ) ) ;
#8696 = EDGE_CURVE ( 'NONE', #1632, #21124, #18358, .T. ) ;
#8697 = PERSON_AND_ORGANIZATION ( #11966, #8758 ) ;
#8699 = EDGE_CURVE ( 'NONE', #14649, #3226, #4471, .T. ) ;
#8698 = VERTEX_POINT ( 'NONE', #13499 ) ;
#8700 = ORIENTED_EDGE ( 'NONE', *, *, #16450, .F. ) ;
#8701 = DIRECTION ( 'NONE',  ( -0.9730401042858024541, 0.2306359803922080898, 5.959266323858942451E-17 ) ) ;
#8702 = FACE_BOUND ( 'NONE', #19882, .T. ) ;
#8703 = DIRECTION ( 'NONE',  ( -0.2306359803922083396, -0.9730401042858023430, 2.222614453595284847E-13 ) ) ;
#8704 = PERSON_AND_ORGANIZATION_ROLE ( 'design_owner' ) ;
#8705 = LINE ( 'NONE', #13820, #13021 ) ;
#8706 = DIRECTION ( 'NONE',  ( -0.2306359803922080343, -0.9730401042858022320, 3.554125915991511201E-14 ) ) ;
#8707 = DIRECTION ( 'NONE',  ( 0.000000000000000000, 0.000000000000000000, 1.000000000000000000 ) ) ;
#8708 = APPROVAL_PERSON_ORGANIZATION ( #6036, #4295, #2355 ) ;
#8709 = AXIS2_PLACEMENT_3D ( 'NONE', #15930, #17840, #12157 ) ;
#8710 = CARTESIAN_POINT ( 'NONE',  ( -23.50000000000000000, -20.00000000000000000, 2.500000000000000000 ) ) ;
#8711 = CALENDAR_DATE ( 2026, 31, 10 ) ;
#8712 = CARTESIAN_POINT ( 'NONE',  ( 37.65496927852454689, 9.564447054075163379, 8.996924156394143779 ) ) ;
#8713 = CARTESIAN_POINT ( 'NONE',  ( 35.09747506357100377, 11.43410645592840069, -27.69000000000049866 ) ) ;
#8714 = CARTESIAN_POINT ( 'NONE',  ( -17.50000000000000000, -20.00000000000000000, 5.000000000000000000 ) ) ;
#8715 = DIRECTION ( 'NONE',  ( -0.9730401042858020100, 0.2306359803922092278, -1.869849304631841307E-15 ) ) ;
#8716 = CARTESIAN_POINT ( 'NONE',  ( -14.54830929633820169, -2.787889851644860251, 5.500000000004459544 ) ) ;
#8717 = ORIENTED_EDGE ( 'NONE', *, *, #2548, .T. ) ;
#8718 = CARTESIAN_POINT ( 'NONE',  ( -18.05391955182270181, 22.49081825942809942, -2.500000000000000000 ) ) ;
#8719 = PRODUCT_DEFINITION_SHAPE ( 'NONE', 'NONE',  #4231 ) ;
#8720 = ORIENTED_EDGE ( 'NONE', *, *, #15064, .F. ) ;
#8721 = CYLINDRICAL_SURFACE ( 'NONE', #12996, 3.499999999999999556 ) ;
#8722 = DIRECTION ( 'NONE',  ( -0.1153179901961009640, -0.4865200521429018377, -0.8660254037844385966 ) ) ;
#8723 = AXIS2_PLACEMENT_3D ( 'NONE', #10526, #1466, #5389 ) ;
#8724 = ORIENTED_EDGE ( 'NONE', *, *, #7613, .F. ) ;
#8725 = CIRCLE ( 'NONE', #20081, 2.499999999999999112 ) ;
#8726 = DIRECTION ( 'NONE',  ( -0.4865200521429014491, 0.1153179901961012555, 0.8660254037844388186 ) ) ;
#8727 = ORIENTED_EDGE ( 'NONE', *, *, #4318, .T. ) ;
#8728 = CARTESIAN_POINT ( 'NONE',  ( -62.91249983789201394, 7.670697574599229185, 2.999765877365274225 ) ) ;
#8729 = AXIS2_PLACEMENT_3D ( 'NONE', #6457, #8603, #14055 ) ;
#8730 = PERSON_AND_ORGANIZATION ( #11966, #8758 ) ;
#8731 = CARTESIAN_POINT ( 'NONE',  ( 30.84445860938240003, -2.459566909556699876, -8.750000000000399680 ) ) ;
#8732 = EDGE_CURVE ( 'NONE', #13324, #6621, #13261, .T. ) ;
#8733 = LINE ( 'NONE', #15745, #3893 ) ;
#8734 = DIRECTION ( 'NONE',  ( 3.210834492181045054E-17, -2.441916418604790135E-15, -1.000000000000000000 ) ) ;
#8735 = APPLICATION_PROTOCOL_DEFINITION ( 'international standard', 'config_control_design', 1994, #20351 ) ;
#8736 = APPROVAL_PERSON_ORGANIZATION ( #19598, #574, #1305 ) ;
#8737 = FACE_OUTER_BOUND ( 'NONE', #1289, .T. ) ;
#8738 = EDGE_LOOP ( 'NONE', ( #23306, #19698, #8506, #15844 ) ) ;
#8739 = CARTESIAN_POINT ( 'NONE',  ( 37.14513723987899851, -6.299761344113198547, -13.00000000000000000 ) ) ;
#8740 = VECTOR ( 'NONE', #17753, 1000.000000000000000 ) ;
#8741 = DESIGN_CONTEXT ( 'detailed design', #2791, 'design' ) ;
#8742 = CARTESIAN_POINT ( 'NONE',  ( -18.05391955182270181, 22.49081825942809942, -4.900728725074969882E-15 ) ) ;
#8743 = ORIENTED_EDGE ( 'NONE', *, *, #12309, .F. ) ;
#8744 = CARTESIAN_POINT ( 'NONE',  ( 34.74610186630083319, 11.66463240636609555, -8.849039310734035269 ) ) ;
#8745 = CARTESIAN_POINT ( 'NONE',  ( -26.99999999999959854, -31.09999999999999787, -21.50000000000000000 ) ) ;
#8746 = VECTOR ( 'NONE', #7747, 1000.000000000000114 ) ;
#8747 = EDGE_LOOP ( 'NONE', ( #12701, #20329, #11658, #20259 ) ) ;
#8748 = PERSON_AND_ORGANIZATION ( #16159, #20904 ) ;
#8749 = DIRECTION ( 'NONE',  ( -1.000000000000000000, -4.040376328279780192E-15, -6.123237831918399306E-17 ) ) ;
#8750 = VECTOR ( 'NONE', #10390, 1000.000000000000227 ) ;
#8751 = EDGE_LOOP ( 'NONE', ( #13244, #19335, #2320, #21920 ) ) ;
#8752 = VERTEX_POINT ( 'NONE', #11627 ) ;
#8753 = PERSON_AND_ORGANIZATION ( #11966, #8758 ) ;
#8754 = CARTESIAN_POINT ( 'NONE',  ( 34.89491389100810181, 23.30074776265909975, -13.00000000000049916 ) ) ;
#8755 = VERTEX_POINT ( 'NONE', #18963 ) ;
#8756 = LOCAL_TIME ( 14, 11, 27.00000000000000000, #7845 ) ;
#8757 = DIRECTION ( 'NONE',  ( -1.000000000000000000, 0.000000000000000000, 0.000000000000000000 ) ) ;
#8758 = ORGANIZATION ( 'UNSPECIFIED', 'UNSPECIFIED', '' ) ;
#8759 = DATE_TIME_ROLE ( 'creation_date' ) ;
#8760 = EDGE_CURVE ( 'NONE', #11069, #11256, #18550, .T. ) ;
#8761 = ADVANCED_FACE ( 'NONE', ( #1248 ), #13420, .T. ) ;
#8762 = PERSON_AND_ORGANIZATION_ROLE ( 'classification_officer' ) ;
#8763 = DIRECTION ( 'NONE',  ( -3.099353312215989243E-62, -1.872670541876879671E-92, 1.000000000000000000 ) ) ;
#8764 = AXIS2_PLACEMENT_3D ( 'NONE', #6677, #17467, #21256 ) ;
#8765 = PLANE ( 'NONE',  #8100 ) ;
#8766 = EDGE_LOOP ( 'NONE', ( #9576, #19312, #13989, #5586 ) ) ;
#8767 = EDGE_CURVE ( 'NONE', #16965, #10063, #14178, .T. ) ;
#8768 = EDGE_CURVE ( 'NONE', #18548, #19937, #15749, .T. ) ;
#8769 = LOCAL_TIME ( 14, 11, 27.00000000000000000, #16250 ) ;
#8770 = VERTEX_POINT ( 'NONE', #20975 ) ;
#8771 = SECURITY_CLASSIFICATION ( '', '', #12745 ) ;
#8772 = DIRECTION ( 'NONE',  ( 1.187319687680494078E-16, 2.805478249478275539E-20, 1.000000000000000000 ) ) ;
#8773 = LINE ( 'NONE', #6879, #2543 ) ;
#8774 = EDGE_LOOP ( 'NONE', ( #9345, #16507, #3064, #16861 ) ) ;
#8775 = VECTOR ( 'NONE', #22747, 1000.000000000000227 ) ;
#8776 = CARTESIAN_POINT ( 'NONE',  ( -25.44839750738890061, 25.46504853262640111, -3.750000000000069722 ) ) ;
#8777 = DIRECTION ( 'NONE',  ( 0.9822591002358885826, -0.1875288244611549582, 5.059610138265688673E-16 ) ) ;
#8778 = ORIENTED_EDGE ( 'NONE', *, *, #7696, .F. ) ;
#8779 = SECURITY_CLASSIFICATION ( '', '', #10330 ) ;
#8780 = VERTEX_POINT ( 'NONE', #17416 ) ;
#8781 = VECTOR ( 'NONE', #18834, 1000.000000000000000 ) ;
#8782 = PERSON_AND_ORGANIZATION ( #11966, #8758 ) ;
#8783 = PERSON ( 'NAUO-PER18', 'UNSPECIFIED', 'UNSPECIFIED', ('UNSPECIFIED'), ('UNSPECIFIED'), ('UNSPECIFIED') ) ;
#8784 = ORIENTED_EDGE ( 'NONE', *, *, #2230, .T. ) ;
#8785 = ORIENTED_EDGE ( 'NONE', *, *, #2548, .F. ) ;
#8786 = CARTESIAN_POINT ( 'NONE',  ( -16.50000000000000000, -20.00000000000000000, 0.000000000000000000 ) ) ;
#8787 = PERSON_AND_ORGANIZATION ( #11966, #8758 ) ;
#8788 = ADVANCED_FACE ( 'NONE', ( #23085, #12207 ), #1123, .T. ) ;
#8789 = APPROVAL_PERSON_ORGANIZATION ( #8535, #15767, #15991 ) ;
#8790 = DIRECTION ( 'NONE',  ( -0.2306359803922033991, -0.9730401042858033422, 0.000000000000000000 ) ) ;
#8791 = DATE_AND_TIME ( #22479, #10243 ) ;
#8792 = AXIS2_PLACEMENT_3D ( 'NONE', #3783, #18296, #2019 ) ;
#8793 = CC_DESIGN_PERSON_AND_ORGANIZATION_ASSIGNMENT ( #20027, #7337, ( #14124 ) ) ;
#8794 = PRODUCT_RELATED_PRODUCT_CATEGORY ( 'detail', '', ( #21034 ) ) ;
#8795 = LOCAL_TIME ( 14, 11, 27.00000000000000000, #21804 ) ;
#8796 = CARTESIAN_POINT ( 'NONE',  ( 26.11627841292220253, -8.532812502301538871, 20.00000000000000000 ) ) ;
#8797 = ADVANCED_FACE ( 'NONE', ( #4819 ), #12428, .F. ) ;
#8798 = EDGE_CURVE ( 'NONE', #1544, #2378, #10033, .T. ) ;
#8799 = APPROVAL_DATE_TIME ( #14138, #4067 ) ;
#8800 = EDGE_CURVE ( 'NONE', #6499, #134, #15627, .T. ) ;
#8801 = ADVANCED_FACE ( 'NONE', ( #5168 ), #10072, .F. ) ;
#8802 = EDGE_LOOP ( 'NONE', ( #5581, #15519, #18650, #1726, #20890 ) ) ;
#8803 = DIRECTION ( 'NONE',  ( -1.000000000000000000, 0.000000000000000000, 0.000000000000000000 ) ) ;
#8804 = EDGE_CURVE ( 'NONE', #4537, #19075, #10192, .T. ) ;
#8805 = DIRECTION ( 'NONE',  ( 0.000000000000000000, 1.000000000000000000, 0.000000000000000000 ) ) ;
#8806 = ORIENTED_EDGE ( 'NONE', *, *, #23469, .F. ) ;
#8807 = EDGE_CURVE ( 'NONE', #11767, #8608, #21010, .T. ) ;
#8808 = LOCAL_TIME ( 14, 11, 27.00000000000000000, #13658 ) ;
#8809 = PLANE ( 'NONE',  #263 ) ;
#8810 = CARTESIAN_POINT ( 'NONE',  ( 33.27836309399499015, 10.32372331478701533, 29.25000000000000000 ) ) ;
#8811 = DIRECTION ( 'NONE',  ( 0.000000000000000000, 1.000000000000000000, 0.000000000000000000 ) ) ;
#8812 = ORIENTED_EDGE ( 'NONE', *, *, #7871, .T. ) ;
#8813 = ORIENTED_EDGE ( 'NONE', *, *, #23166, .T. ) ;
#8814 = CARTESIAN_POINT ( 'NONE',  ( -0.5391976746803449627, 18.33937061236850141, -7.621247264287879719E-15 ) ) ;
#8815 = PERSON_AND_ORGANIZATION_ROLE ( 'design_owner' ) ;
#8816 = VERTEX_POINT ( 'NONE', #3034 ) ;
#8817 = AXIS2_PLACEMENT_3D ( 'NONE', #11643, #13404, #2701 ) ;
#8818 = ORIENTED_EDGE ( 'NONE', *, *, #1526, .T. ) ;
#8819 = DIRECTION ( 'NONE',  ( 1.000000000000000000, 0.000000000000000000, 1.480297366166879989E-16 ) ) ;
#8820 = AXIS2_PLACEMENT_3D ( 'NONE', #5757, #166, #19783 ) ;
#8821 = CARTESIAN_POINT ( 'NONE',  ( 31.01827548281339020, -2.500766059351007708, 11.00000000000020428 ) ) ;
#8822 = CC_DESIGN_SECURITY_CLASSIFICATION ( #17915, ( #23510 ) ) ;
#8823 = DIRECTION ( 'NONE',  ( 0.8633955506089426857, 0.5045276238113038936, 1.318113719833497156E-16 ) ) ;
#8824 = COORDINATED_UNIVERSAL_TIME_OFFSET ( 0, 0, .AHEAD. ) ;
#8825 = PLANE ( 'NONE',  #8602 ) ;
#8826 = VECTOR ( 'NONE', #988, 1000.000000000000000 ) ;
#8827 = EDGE_CURVE ( 'NONE', #20679, #21354, #16092, .T. ) ;
#8828 = FACE_BOUND ( 'NONE', #18665, .T. ) ;
#8829 = AXIS2_PLACEMENT_3D ( 'NONE', #17728, #21159, #11941 ) ;
#8830 = PRODUCT_DEFINITION_FORMATION_WITH_SPECIFIED_SOURCE ( 'ANY', '', #13107, .NOT_KNOWN. ) ;
#8831 = DIRECTION ( 'NONE',  ( 1.000000000000000000, 0.000000000000000000, 0.000000000000000000 ) ) ;
#8832 = AXIS2_PLACEMENT_3D ( 'NONE', #21152, #3222, #22571 ) ;
#8833 = ADVANCED_FACE ( 'NONE', ( #8737 ), #11568, .F. ) ;
#8834 = VECTOR ( 'NONE', #6603, 1000.000000000000114 ) ;
#8835 = EDGE_CURVE ( 'NONE', #3556, #17992, #13853, .T. ) ;
#8836 = LINE ( 'NONE', #1686, #13213 ) ;
#8837 = DATE_TIME_ROLE ( 'creation_date' ) ;
#8838 = CONICAL_SURFACE ( 'NONE', #9216, 2.283500000000000085, 0.7853981633974469467 ) ;
#8839 =( BOUNDED_CURVE ( )  B_SPLINE_CURVE ( 2, ( #7518, #713, #22330 ),
 .UNSPECIFIED., .F., .F. ) 
 B_SPLINE_CURVE_WITH_KNOTS ( ( 3, 3 ),
 ( 0.000000000000000000, 0.2928548593876180162 ),
 .UNSPECIFIED. ) 
 CURVE ( )  GEOMETRIC_REPRESENTATION_ITEM ( )  RATIONAL_B_SPLINE_CURVE ( ( 1.000000000000000000, 1.037954849302029858, 1.000000000000000000 ) ) 
 REPRESENTATION_ITEM ( '' )  );
#8840 = CARTESIAN_POINT ( 'NONE',  ( 113.2956221386590130, -28.78551670568849730, 2.700000000000000178 ) ) ;
#8841 = CARTESIAN_POINT ( 'NONE',  ( 29.27674327513866004, 1.765923432495573264, -13.00000000000039968 ) ) ;
#8842 = VECTOR ( 'NONE', #15955, 1000.000000000000000 ) ;
#8843 = CARTESIAN_POINT ( 'NONE',  ( -62.91249983789198552, 7.670697574599230073, 2.108981951733699973E-15 ) ) ;
#8844 = LINE ( 'NONE', #139, #7109 ) ;
#8845 = DIRECTION ( 'NONE',  ( -0.2306359803922033713, -0.9730401042858033422, 5.180237729619581644E-15 ) ) ;
#8846 = ORIENTED_EDGE ( 'NONE', *, *, #8568, .F. ) ;
#8847 = DIRECTION ( 'NONE',  ( -0.9730401042858035643, 0.2306359803922028717, -2.804983810440358308E-16 ) ) ;
#8848 = CC_DESIGN_APPROVAL ( #651, ( #19087 ) ) ;
#8849 = ORIENTED_EDGE ( 'NONE', *, *, #5564, .T. ) ;
#8850 = CARTESIAN_POINT ( 'NONE',  ( 120.8697533057606961, 5.046729969097192736, -13.00000000000000000 ) ) ;
#8851 = DIRECTION ( 'NONE',  ( -6.123230174520380038E-17, -4.962644601432250805E-15, -1.000000000000000000 ) ) ;
#8852 = ORIENTED_EDGE ( 'NONE', *, *, #2508, .F. ) ;
#8853 = AXIS2_PLACEMENT_3D ( 'NONE', #15191, #21950, #13429 ) ;
#8854 = CIRCLE ( 'NONE', #5812, 7.000000000000000000 ) ;
#8855 = LINE ( 'NONE', #12412, #842 ) ;
#8857 = VERTEX_POINT ( 'NONE', #19197 ) ;
#8856 = EDGE_CURVE ( 'NONE', #3741, #17116, #138, .T. ) ;
#8858 = AXIS2_PLACEMENT_3D ( 'NONE', #4673, #2886, #10148 ) ;
#8859 = CARTESIAN_POINT ( 'NONE',  ( 35.59419854219520118, 9.774809681453278998, -27.87500000000050093 ) ) ;
#8860 = DATE_AND_TIME ( #21311, #17972 ) ;
#8861 = FACE_OUTER_BOUND ( 'NONE', #2815, .T. ) ;
#8862 = ADVANCED_FACE ( 'NONE', ( #17766 ), #2923, .T. ) ;
#8863 = TOROIDAL_SURFACE ( 'NONE', #13791, 2.700000000000000178, 0.2000000000000000111 ) ;
#8864 = CARTESIAN_POINT ( 'NONE',  ( -62.82872441665799101, -8.329083101359751495, -7.727128097349530051E-15 ) ) ;
#8865 = EDGE_CURVE ( 'NONE', #21144, #3898, #15860, .T. ) ;
#8866 = DIRECTION ( 'NONE',  ( 0.000000000000000000, 0.000000000000000000, -1.000000000000000000 ) ) ;
#8867 =( LENGTH_UNIT ( ) NAMED_UNIT ( * ) SI_UNIT ( .MILLI., .METRE. ) );
#8868 = LOCAL_TIME ( 14, 11, 27.00000000000000000, #23432 ) ;
#8869 = VECTOR ( 'NONE', #14456, 1000.000000000000000 ) ;
#8870 = EDGE_CURVE ( 'NONE', #19293, #18213, #1473, .T. ) ;
#8871 = DIRECTION ( 'NONE',  ( 0.2306359803922028162, 0.9730401042858035643, -1.412237191019910621E-17 ) ) ;
#8872 =( REPRESENTATION_RELATIONSHIP ('NONE','NONE', #18121, #22194 ) REPRESENTATION_RELATIONSHIP_WITH_TRANSFORMATION ( #16595 )SHAPE_REPRESENTATION_RELATIONSHIP( ) );
#8873 = CIRCLE ( 'NONE', #10410, 0.5000000000000004441 ) ;
#8874 = DIRECTION ( 'NONE',  ( -0.9730401042858024541, 0.2306359803922080898, 5.959266323858942451E-17 ) ) ;
#8875 = DIRECTION ( 'NONE',  ( 0.2306359803922025109, 0.9730401042858035643, -5.112869192352692394E-15 ) ) ;
#8876 = CIRCLE ( 'NONE', #1276, 0.5000000000000000000 ) ;
#8877 = CARTESIAN_POINT ( 'NONE',  ( 114.8732178155626826, -20.25231274233364687, 13.00000000000000000 ) ) ;
#8878 = EDGE_LOOP ( 'NONE', ( #13461, #6400, #15152, #13059 ) ) ;
#8879 = DIRECTION ( 'NONE',  ( 0.9730401042858036753, -0.2306359803922031493, -5.959266323858673745E-17 ) ) ;
#8880 = FACE_BOUND ( 'NONE', #13533, .T. ) ;
#8881 = ORIENTED_EDGE ( 'NONE', *, *, #16658, .F. ) ;
#8882 = CALENDAR_DATE ( 2026, 31, 10 ) ;
#8883 = CARTESIAN_POINT ( 'NONE',  ( 118.5079952955230027, -6.794810348829379620, -15.90000000000000036 ) ) ;
#8884 = EDGE_LOOP ( 'NONE', ( #20548, #20449, #16984 ) ) ;
#8885 = CONICAL_SURFACE ( 'NONE', #18294, 2.283499999999998753, 0.7853981633974433940 ) ;
#8886 = ORIENTED_EDGE ( 'NONE', *, *, #2108, .F. ) ;
#8887 = APPROVAL_STATUS ( 'not_yet_approved' ) ;
#8888 = DIRECTION ( 'NONE',  ( -0.9730401042858022320, 0.2306359803922080343, 5.959266323858941219E-17 ) ) ;
#8889 = ORIENTED_EDGE ( 'NONE', *, *, #12309, .T. ) ;
#8890 = DIRECTION ( 'NONE',  ( -4.328311834315510110E-15, -1.851928590941880236E-14, 1.000000000000000000 ) ) ;
#8891 = APPLICATION_PROTOCOL_DEFINITION ( 'international standard', 'config_control_design', 1994, #20492 ) ;
#8892 = CIRCLE ( 'NONE', #7739, 2.066999999999998394 ) ;
#8893 = PRODUCT_RELATED_PRODUCT_CATEGORY ( 'detail', '', ( #1104 ) ) ;
#8894 = COORDINATED_UNIVERSAL_TIME_OFFSET ( 0, 0, .AHEAD. ) ;
#8895 = CARTESIAN_POINT ( 'NONE',  ( 1.836479826415680084E-19, -7.772252928343919938E-16, -8.889558542813568797E-14 ) ) ;
#8896 = DIRECTION ( 'NONE',  ( 0.2306359803922080898, 0.9730401042858024541, -2.572202231434325988E-16 ) ) ;
#8897 = ORIENTED_EDGE ( 'NONE', *, *, #8964, .F. ) ;
#8898 = CARTESIAN_POINT ( 'NONE',  ( -0.03403376487617929685, 6.499910899608420500, 8.874490886070419291E-14 ) ) ;
#8899 = ORIENTED_EDGE ( 'NONE', *, *, #1508, .T. ) ;
#8900 = CARTESIAN_POINT ( 'NONE',  ( 35.35837847849400362, 22.00420084508159846, 15.00000000000000000 ) ) ;
#8901 = FACE_OUTER_BOUND ( 'NONE', #7441, .T. ) ;
#8902 = ORIENTED_EDGE ( 'NONE', *, *, #12310, .F. ) ;
#8903 = EDGE_CURVE ( 'NONE', #12330, #12414, #5519, .T. ) ;
#8904 = FACE_OUTER_BOUND ( 'NONE', #20203, .T. ) ;
#8905 = CARTESIAN_POINT ( 'NONE',  ( -62.93867965702761325, 12.67062903583649991, 3.427095671567209849E-15 ) ) ;
#8906 = ORIENTED_EDGE ( 'NONE', *, *, #2167, .T. ) ;
#8907 = VERTEX_POINT ( 'NONE', #20009 ) ;
#8908 = PERSON_AND_ORGANIZATION ( #11966, #8758 ) ;
#8909 = VERTEX_POINT ( 'NONE', #16546 ) ;
#8910 = ORIENTED_EDGE ( 'NONE', *, *, #94, .F. ) ;
#8911 = DIRECTION ( 'NONE',  ( 1.000000000000000000, -8.896220237034308570E-17, 0.000000000000000000 ) ) ;
#8912 = DATE_AND_TIME ( #92, #8060 ) ;
#8913 = EDGE_CURVE ( 'NONE', #1017, #15497, #19899, .T. ) ;
#8914 = CARTESIAN_POINT ( 'NONE',  ( 0.000000000000000000, -17.30000000000000071, -2.500000000000000000 ) ) ;
#8915 = CONTEXT_DEPENDENT_SHAPE_REPRESENTATION ( #10213, #17294 ) ;
#8916 = FACE_OUTER_BOUND ( 'NONE', #1777, .T. ) ;
#8917 = PERSON_AND_ORGANIZATION ( #11966, #8758 ) ;
#8918 = PRODUCT_DEFINITION_SHAPE ( 'NONE', 'NONE',  #19756 ) ;
#8919 = VERTEX_POINT ( 'NONE', #14775 ) ;
#8920 = DIRECTION ( 'NONE',  ( -0.2306359803922053142, -0.9730401042858028982, 0.000000000000000000 ) ) ;
#8921 = EDGE_LOOP ( 'NONE', ( #8326, #21308, #7842, #14062 ) ) ;
#8922 = EDGE_CURVE ( 'NONE', #2801, #341, #5278, .T. ) ;
#8923 = CARTESIAN_POINT ( 'NONE',  ( 43.84419854219520829, -33.09999999999998721, -21.50000000000000000 ) ) ;
#8924 = VECTOR ( 'NONE', #22645, 1000.000000000000000 ) ;
#8925 = CARTESIAN_POINT ( 'NONE',  ( 33.90884364377009774, 10.17428291754599989, -27.69000000000049866 ) ) ;
#8926 = DIRECTION ( 'NONE',  ( 0.005235963827117092427, -0.9999862922474493931, -2.636227439667000721E-16 ) ) ;
#8927 = ORIENTED_EDGE ( 'NONE', *, *, #14857, .T. ) ;
#8928 = ORIENTED_EDGE ( 'NONE', *, *, #15022, .F. ) ;
#8929 = DIRECTION ( 'NONE',  ( 0.2306359803922085339, 0.9730401042858022320, 0.000000000000000000 ) ) ;
#8930 = ORIENTED_EDGE ( 'NONE', *, *, #10909, .F. ) ;
#8931 = CC_DESIGN_DATE_AND_TIME_ASSIGNMENT ( #5623, #264, ( #18743 ) ) ;
#8932 = DATE_TIME_ROLE ( 'classification_date' ) ;
#8933 = VERTEX_POINT ( 'NONE', #20123 ) ;
#8934 = VERTEX_POINT ( 'NONE', #16437 ) ;
#8935 = CARTESIAN_POINT ( 'NONE',  ( 30.84445860938240003, -2.459566909556570202, 13.00000000000019895 ) ) ;
#8936 = DIRECTION ( 'NONE',  ( -1.751019220569994795E-16, -2.300154215587015208E-15, -1.000000000000000000 ) ) ;
#8937 = CARTESIAN_POINT ( 'NONE',  ( 31.45181451370270054, 16.90945435098589655, -25.00000000000000000 ) ) ;
#8938 = APPROVAL_DATE_TIME ( #22089, #10684 ) ;
#8939 = EDGE_CURVE ( 'NONE', #12850, #3176, #13442, .T. ) ;
#8940 = CARTESIAN_POINT ( 'NONE',  ( 114.2412296582679971, -24.79605227811680379, 3.000000000000000000 ) ) ;
#8941 = ADVANCED_FACE ( 'NONE', ( #11002 ), #18229, .T. ) ;
#8942 = CARTESIAN_POINT ( 'NONE',  ( 36.17078849317569933, 12.20740994216779107, -26.30000000000050875 ) ) ;
#8943 = AXIS2_PLACEMENT_3D ( 'NONE', #19569, #14682, #1973 ) ;
#8944 = DIRECTION ( 'NONE',  ( 1.000000000000000000, 0.000000000000000000, 0.000000000000000000 ) ) ;
#8945 = DIRECTION ( 'NONE',  ( 0.9579954394086682701, 0.2867834340965191298, -1.451283422213149430E-15 ) ) ;
#8946 = PERSON_AND_ORGANIZATION ( #11966, #8758 ) ;
#8947 = DIRECTION ( 'NONE',  ( 3.099353312215989243E-62, -1.534091707905539548E-92, -1.000000000000000000 ) ) ;
#8948 = CARTESIAN_POINT ( 'NONE',  ( -59.87132660632070014, -21.81388311970430038, -5.000000000000000000 ) ) ;
#8949 = CARTESIAN_POINT ( 'NONE',  ( 1.213484035536889882, 25.73383521926719908, 2.500000000000000000 ) ) ;
#8950 = ADVANCED_FACE ( 'NONE', ( #10895 ), #5403, .F. ) ;
#8951 = FACE_OUTER_BOUND ( 'NONE', #492, .T. ) ;
#8952 = LINE ( 'NONE', #3603, #444 ) ;
#8953 = ORIENTED_EDGE ( 'NONE', *, *, #1683, .T. ) ;
#8954 = LINE ( 'NONE', #10984, #14513 ) ;
#8955 = UNCERTAINTY_MEASURE_WITH_UNIT (LENGTH_MEASURE( 1.000000000000000082E-05 ), #5114, 'distance_accuracy_value', 'NONE');
#8956 = CC_DESIGN_PERSON_AND_ORGANIZATION_ASSIGNMENT ( #15326, #472, ( #13165 ) ) ;
#8957 = PRODUCT_DEFINITION ( 'UNKNOWN', '', #22008, #22743 ) ;
#8958 = VERTEX_POINT ( 'NONE', #3730 ) ;
#8959 = DIRECTION ( 'NONE',  ( -6.193954341422139021E-17, -4.965628413872130537E-15, -1.000000000000000000 ) ) ;
#8960 = DIRECTION ( 'NONE',  ( -1.000000000000000000, 0.000000000000000000, 1.159535895544890222E-14 ) ) ;
#8961 = ORIENTED_EDGE ( 'NONE', *, *, #12135, .T. ) ;
#8962 = EDGE_CURVE ( 'NONE', #20542, #199, #11937, .T. ) ;
#8963 = PLANE ( 'NONE',  #17188 ) ;
#8964 = EDGE_CURVE ( 'NONE', #20644, #19182, #9320, .T. ) ;
#8965 = AXIS2_PLACEMENT_3D ( 'NONE', #7585, #5814, #16256 ) ;
#8966 = ORIENTED_EDGE ( 'NONE', *, *, #6628, .T. ) ;
#8967 = DIRECTION ( 'NONE',  ( 1.138590270679730064E-14, 2.220446049251245514E-15, 1.000000000000000000 ) ) ;
#8968 = DATE_AND_TIME ( #10772, #10389 ) ;
#8969 = LINE ( 'NONE', #1468, #6744 ) ;
#8970 = FACE_OUTER_BOUND ( 'NONE', #19238, .T. ) ;
#8971 = FACE_OUTER_BOUND ( 'NONE', #23123, .T. ) ;
#8972 = PERSON_AND_ORGANIZATION ( #11966, #8758 ) ;
#8973 = VECTOR ( 'NONE', #7116, 1000.000000000000000 ) ;
#8974 = VECTOR ( 'NONE', #15416, 1000.000000000000000 ) ;
#8975 = DIRECTION ( 'NONE',  ( 0.000000000000000000, 0.000000000000000000, -1.000000000000000000 ) ) ;
#8976 = CARTESIAN_POINT ( 'NONE',  ( -14.00000000397270128, 22.95208919312850071, 8.000000000004400036 ) ) ;
#8977 = LINE ( 'NONE', #7088, #8198 ) ;
#8978 = ADVANCED_FACE ( 'NONE', ( #18359 ), #11126, .F. ) ;
#8979 = DIRECTION ( 'NONE',  ( 0.2306359803922028995, 0.9730401042858035643, -4.741332172907957521E-18 ) ) ;
#8980 = VERTEX_POINT ( 'NONE', #18007 ) ;
#8981 = CARTESIAN_POINT ( 'NONE',  ( 2.500000000000026645, -7.535786464196452844E-15, 5.000000000000000000 ) ) ;
#8982 = DIRECTION ( 'NONE',  ( -0.6988463228792121118, -0.7152718483193672983, -1.324025346201481692E-16 ) ) ;
#8983 = ORIENTED_EDGE ( 'NONE', *, *, #16245, .T. ) ;
#8984 = EDGE_CURVE ( 'NONE', #11278, #5941, #4338, .T. ) ;
#8985 = EDGE_CURVE ( 'NONE', #9873, #18882, #1829, .T. ) ;
#8986 = DATE_AND_TIME ( #6856, #21640 ) ;
#8987 = CARTESIAN_POINT ( 'NONE',  ( 39.37089837072280574, 22.23982225285502068, -10.50000000000049916 ) ) ;
#8988 = ORIENTED_EDGE ( 'NONE', *, *, #6612, .F. ) ;
#8989 = APPLICATION_CONTEXT ( 'configuration controlled 3d designs of mechanical parts and assemblies' ) ;
#8990 = ADVANCED_FACE ( 'NONE', ( #17880, #5750 ), #3378, .F. ) ;
#8991 = DATE_AND_TIME ( #19790, #1939 ) ;
#8992 = DIRECTION ( 'NONE',  ( -1.159535895544890222E-14, -2.167612681253619929E-15, -1.000000000000000000 ) ) ;
#8993 = ORIENTED_EDGE ( 'NONE', *, *, #19519, .T. ) ;
#8994 = VECTOR ( 'NONE', #6138, 1000.000000000000114 ) ;
#8995 = EDGE_CURVE ( 'NONE', #12330, #19270, #12539, .T. ) ;
#8996 = AXIS2_PLACEMENT_3D ( 'NONE', #18152, #3652, #3546 ) ;
#8997 = CARTESIAN_POINT ( 'NONE',  ( -20.00000000000000000, -20.00000000000000000, -2.500000000000000000 ) ) ;
#8998 = CIRCLE ( 'NONE', #21871, 2.500000000028978597 ) ;
#8999 = COORDINATED_UNIVERSAL_TIME_OFFSET ( 0, 0, .AHEAD. ) ;
#9000 = CALENDAR_DATE ( 2026, 31, 10 ) ;
#9001 = LINE ( 'NONE', #16234, #21442 ) ;
#9002 = AXIS2_PLACEMENT_3D ( 'NONE', #20569, #22463, #11579 ) ;
#9003 = DIRECTION ( 'NONE',  ( 0.000000000000000000, 0.000000000000000000, 1.000000000000000000 ) ) ;
#9004 = ORIENTED_EDGE ( 'NONE', *, *, #14345, .T. ) ;
#9005 = DIRECTION ( 'NONE',  ( -1.000000000000000000, -1.296622928517386003E-46, 0.000000000000000000 ) ) ;
#9006 = AXIS2_PLACEMENT_3D ( 'NONE', #22825, #20931, #20590 ) ;
#9007 = VECTOR ( 'NONE', #5342, 1000.000000000000000 ) ;
#9008 = ORIENTED_EDGE ( 'NONE', *, *, #1827, .F. ) ;
#9009 = DIRECTION ( 'NONE',  ( -0.9997648975362222190, -0.02168293463503410262, 0.000000000000000000 ) ) ;
#9010 = CARTESIAN_POINT ( 'NONE',  ( -14.00000000000180123, -19.99999999944489915, -7.999999999996829203 ) ) ;
#9011 = ORIENTED_EDGE ( 'NONE', *, *, #18938, .T. ) ;
#9012 = CC_DESIGN_DATE_AND_TIME_ASSIGNMENT ( #3440, #19490, ( #7977 ) ) ;
#9013 = CYLINDRICAL_SURFACE ( 'NONE', #5394, 2.500000000000000888 ) ;
#9014 = CARTESIAN_POINT ( 'NONE',  ( -2.500000000000012434, -17.29999999999999361, 5.000000000000000000 ) ) ;
#9015 = AXIS2_PLACEMENT_3D ( 'NONE', #973, #15587, #11947 ) ;
#9016 = ORIENTED_EDGE ( 'NONE', *, *, #11385, .F. ) ;
#9017 = DATE_AND_TIME ( #1516, #34 ) ;
#9018 = VERTEX_POINT ( 'NONE', #19775 ) ;
#9019 = EDGE_LOOP ( 'NONE', ( #16266, #2690, #17313, #2351 ) ) ;
#9020 = DIRECTION ( 'NONE',  ( -0.005235963827104182615, 0.9999862922474495042, 5.936218956635594600E-19 ) ) ;
#9021 = CIRCLE ( 'NONE', #15444, 7.000000000000000000 ) ;
#9022 = APPROVAL_STATUS ( 'not_yet_approved' ) ;
#9023 = CIRCLE ( 'NONE', #16221, 49.22658835543908395 ) ;
#9024 = AXIS2_PLACEMENT_3D ( 'NONE', #20181, #22944, #14483 ) ;
#9025 = CARTESIAN_POINT ( 'NONE',  ( 35.59419854219520118, 9.774809681453278998, 23.00000000000000000 ) ) ;
#9026 = AXIS2_PLACEMENT_3D ( 'NONE', #5164, #23324, #7082 ) ;
#9027 = LINE ( 'NONE', #16258, #1707 ) ;
#9028 = EDGE_CURVE ( 'NONE', #22900, #11749, #23441, .T. ) ;
#9029 = DIRECTION ( 'NONE',  ( -1.000000000000000000, 0.000000000000000000, 0.000000000000000000 ) ) ;
#9030 = PERSON_AND_ORGANIZATION ( #11966, #8758 ) ;
#9031 = ORIENTED_EDGE ( 'NONE', *, *, #17769, .F. ) ;
#9032 = AXIS2_PLACEMENT_3D ( 'NONE', #16684, #8155, #13257 ) ;
#9033 = DIRECTION ( 'NONE',  ( -0.2306359803922080343, -0.9730401042858022320, 5.076717492620541185E-14 ) ) ;
#9034 = DIRECTION ( 'NONE',  ( 0.9730401042858035643, -0.2306359803922028717, -5.959266323858677443E-17 ) ) ;
#9035 = EDGE_LOOP ( 'NONE', ( #14811, #22054, #1490, #1018 ) ) ;
#9036 = DIRECTION ( 'NONE',  ( 0.2306359803922080343, 0.9730401042858022320, -2.572202231434325495E-16 ) ) ;
#9037 = CYLINDRICAL_SURFACE ( 'NONE', #22498, 6.499999999999997335 ) ;
#9038 = DIRECTION ( 'NONE',  ( -0.9997651245102238127, -0.02167246670447303680, 0.000000000000000000 ) ) ;
#9039 = ORIENTED_EDGE ( 'NONE', *, *, #23080, .F. ) ;
#9040 = ORIENTED_EDGE ( 'NONE', *, *, #118, .F. ) ;
#9041 = DIRECTION ( 'NONE',  ( 0.000000000000000000, 0.000000000000000000, -1.000000000000000000 ) ) ;
#9042 = ORIENTED_EDGE ( 'NONE', *, *, #6669, .T. ) ;
#9043 = PERSON_AND_ORGANIZATION ( #11966, #8758 ) ;
#9044 = EDGE_LOOP ( 'NONE', ( #15923, #16553, #6090, #21098 ) ) ;
#9045 = ORIENTED_EDGE ( 'NONE', *, *, #20558, .F. ) ;
#9046 = LINE ( 'NONE', #1674, #16072 ) ;
#9047 = DIRECTION ( 'NONE',  ( 0.1187863113461967018, 0.5011527021216418687, 0.8571673007021100021 ) ) ;
#9048 = COORDINATED_UNIVERSAL_TIME_OFFSET ( 0, 0, .AHEAD. ) ;
#9049 = CARTESIAN_POINT ( 'NONE',  ( 114.9405074087380001, 12.84085624101770051, -2.283499999999970775 ) ) ;
#9050 = CARTESIAN_POINT ( 'NONE',  ( 83.72351314638889619, 11.21323789678963934, 3.777010778495970333E-14 ) ) ;
#9051 = EDGE_CURVE ( 'NONE', #4601, #3018, #19501, .T. ) ;
#9052 = CONICAL_SURFACE ( 'NONE', #2560, 1.033499999999998753, 1.029744258676650093 ) ;
#9053 = CARTESIAN_POINT ( 'NONE',  ( 0.000000000000000000, 0.000000000000000000, 0.000000000000000000 ) ) ;
#9054 = VERTEX_POINT ( 'NONE', #20709 ) ;
#9055 = FACE_OUTER_BOUND ( 'NONE', #7387, .T. ) ;
#9056 = PERSON_AND_ORGANIZATION ( #11966, #8758 ) ;
#9057 = DIRECTION ( 'NONE',  ( -0.9997648975362222190, -0.02168293463503410262, 0.000000000000000000 ) ) ;
#9058 = CARTESIAN_POINT ( 'NONE',  ( 33.90884364377009774, 10.17428291754630010, 27.68999999999999773 ) ) ;
#9059 = ADVANCED_FACE ( 'NONE', ( #7890 ), #11242, .F. ) ;
#9060 = EDGE_CURVE ( 'NONE', #22465, #22663, #22490, .T. ) ;
#9061 = PLANE ( 'NONE',  #16930 ) ;
#9062 = CARTESIAN_POINT ( 'NONE',  ( 35.59419854219520118, 9.774809681453540122, 26.50000000000000000 ) ) ;
#9063 = DIRECTION ( 'NONE',  ( -1.000000000000000000, 0.000000000000000000, 0.000000000000000000 ) ) ;
#9064 = EDGE_LOOP ( 'NONE', ( #5917, #20034, #12212, #12781 ) ) ;
#9065 = DIRECTION ( 'NONE',  ( -0.9730401042858024541, 0.2306359803922080898, 5.959266323858942451E-17 ) ) ;
#9066 = EDGE_LOOP ( 'NONE', ( #14400, #2960, #14726, #7829 ) ) ;
#9067 = CARTESIAN_POINT ( 'NONE',  ( -20.00000000397129796, 22.95208919256900160, 6.500000000004299672 ) ) ;
#9068 = DIRECTION ( 'NONE',  ( 0.005235963827108232327, -0.9999862922474493931, -5.936218956694023463E-19 ) ) ;
#9069 = EDGE_LOOP ( 'NONE', ( #21735, #4308 ) ) ;
#9070 = FACE_OUTER_BOUND ( 'NONE', #5094, .T. ) ;
#9071 = ORIENTED_EDGE ( 'NONE', *, *, #21461, .F. ) ;
#9072 = DIRECTION ( 'NONE',  ( 6.123230174520409620E-17, 4.962644601432260272E-15, 1.000000000000000000 ) ) ;
#9073 = PERSON_AND_ORGANIZATION_ROLE ( 'design_owner' ) ;
#9074 = VECTOR ( 'NONE', #11492, 999.9999999999998863 ) ;
#9075 = CARTESIAN_POINT ( 'NONE',  ( 35.59419854219520118, 9.774809681453559662, 29.25000000000000000 ) ) ;
#9076 = EDGE_CURVE ( 'NONE', #20644, #9363, #7007, .T. ) ;
#9077 = CARTESIAN_POINT ( 'NONE',  ( -60.05196788195259927, 12.68574396146170180, -5.000000000000000000 ) ) ;
#9078 = PRODUCT_DEFINITION ( 'UNKNOWN', '', #19087, #163 ) ;
#9079 = DIRECTION ( 'NONE',  ( -6.662161100567945949E-09, 1.000000000000000000, -2.081668171172169697E-15 ) ) ;
#9080 = PERSON_AND_ORGANIZATION ( #11966, #8758 ) ;
#9081 = CC_DESIGN_PERSON_AND_ORGANIZATION_ASSIGNMENT ( #19446, #2700, ( #18531 ) ) ;
#9082 = DIRECTION ( 'NONE',  ( 3.099353312215989243E-62, 0.000000000000000000, -1.000000000000000000 ) ) ;
#9083 = DIRECTION ( 'NONE',  ( 0.000000000000000000, 0.000000000000000000, -1.000000000000000000 ) ) ;
#9084 = EDGE_CURVE ( 'NONE', #6859, #1745, #5987, .T. ) ;
#9085 = EDGE_CURVE ( 'NONE', #11939, #1307, #5459, .T. ) ;
#9086 = DIRECTION ( 'NONE',  ( -0.2306359803922019835, -0.9730401042858037863, 4.163336342344336238E-15 ) ) ;
#9087 = DIRECTION ( 'NONE',  ( -1.000000000000000000, 2.775557561562891351E-15, 0.000000000000000000 ) ) ;
#9088 = CC_DESIGN_PERSON_AND_ORGANIZATION_ASSIGNMENT ( #23155, #10608, ( #11807 ) ) ;
#9089 = SECURITY_CLASSIFICATION ( '', '', #10824 ) ;
#9090 = CARTESIAN_POINT ( 'NONE',  ( 35.34171762861019772, 30.38879166913039853, -20.00000000000029843 ) ) ;
#9091 = AXIS2_PLACEMENT_3D ( 'NONE', #10038, #17264, #2285 ) ;
#9092 = CARTESIAN_POINT ( 'NONE',  ( 53.15246078658950069, 27.48624099592299785, 3.293763653412249631E-14 ) ) ;
#9093 = ORIENTED_EDGE ( 'NONE', *, *, #11317, .F. ) ;
#9094 = MANIFOLD_SOLID_BREP ( 'Imported1', #15205 ) ;
#9095 = ORIENTED_EDGE ( 'NONE', *, *, #833, .T. ) ;
#9096 = DIRECTION ( 'NONE',  ( 0.005225493778937319485, -0.9999863470141810984, 2.442038948240150648E-15 ) ) ;
#9097 = CARTESIAN_POINT ( 'NONE',  ( 111.8137341348020044, 5.068973512656589797, 13.00000000000000000 ) ) ;
#9098 = ORIENTED_EDGE ( 'NONE', *, *, #20000, .T. ) ;
#9099 = APPLICATION_PROTOCOL_DEFINITION ( 'international standard', 'config_control_design', 1994, #11890 ) ;
#9100 = DIRECTION ( 'NONE',  ( -0.9730401042858024541, 0.2306359803922080898, 5.959266323859082967E-17 ) ) ;
#9101 = VERTEX_POINT ( 'NONE', #631 ) ;
#9102 = DIRECTION ( 'NONE',  ( -1.000000000000000000, 1.982541115402065307E-15, 0.000000000000000000 ) ) ;
#9103 = DATE_AND_TIME ( #7104, #2775 ) ;
#9104 = EDGE_CURVE ( 'NONE', #23466, #5808, #20599, .T. ) ;
#9105 = PRODUCT_DEFINITION_SHAPE ( 'NONE', 'NONE',  #7139 ) ;
#9106 = APPROVAL_PERSON_ORGANIZATION ( #5116, #6205, #19950 ) ;
#9107 = DATE_AND_TIME ( #1849, #8795 ) ;
#9108 = VECTOR ( 'NONE', #21532, 1000.000000000000000 ) ;
#9109 = PLANE ( 'NONE',  #3250 ) ;
#9110 = AXIS2_PLACEMENT_3D ( 'NONE', #5368, #21287, #4 ) ;
#9111 = VECTOR ( 'NONE', #18304, 999.9999999999998863 ) ;
#9112 = DIRECTION ( 'NONE',  ( 0.9730401042858035643, -0.2306359803922028717, -5.432877459303547053E-17 ) ) ;
#9113 = ORIENTED_EDGE ( 'NONE', *, *, #13495, .F. ) ;
#9115 = VECTOR ( 'NONE', #20088, 1000.000000000000114 ) ;
#9114 = FACE_OUTER_BOUND ( 'NONE', #19370, .T. ) ;
#9116 = ADVANCED_FACE ( 'NONE', ( #11358, #15364 ), #8137, .T. ) ;
#9117 = ADVANCED_FACE ( 'NONE', ( #13238 ), #16908, .F. ) ;
#9118 = ORIENTED_EDGE ( 'NONE', *, *, #12647, .T. ) ;
#9119 = CIRCLE ( 'NONE', #13675, 2.650000000000001688 ) ;
#9120 = CARTESIAN_POINT ( 'NONE',  ( -20.00000000397270128, 22.95208919257349933, 5.500000000004459544 ) ) ;
#9121 = CARTESIAN_POINT ( 'NONE',  ( -61.44393618248319910, 13.67846927382480082, -5.515300856952130332E-15 ) ) ;
#9122 = FACE_OUTER_BOUND ( 'NONE', #3795, .T. ) ;
#9123 = ORIENTED_EDGE ( 'NONE', *, *, #3012, .T. ) ;
#9124 = APPLICATION_CONTEXT ( 'configuration controlled 3d designs of mechanical parts and assemblies' ) ;
#9125 = LOCAL_TIME ( 14, 11, 27.00000000000000000, #1898 ) ;
#9126 = ITEM_DEFINED_TRANSFORMATION ( 'NONE', 'NONE', #17048,  #12739 ) ;
#9127 = DIRECTION ( 'NONE',  ( -0.7071067811865475727, 0.000000000000000000, -0.7071067811865475727 ) ) ;
#9128 = ORIENTED_EDGE ( 'NONE', *, *, #1945, .T. ) ;
#9129 = APPROVAL_STATUS ( 'not_yet_approved' ) ;
#9130 = ORIENTED_EDGE ( 'NONE', *, *, #7055, .T. ) ;
#9131 = EDGE_LOOP ( 'NONE', ( #21468, #8743, #21444, #7153 ) ) ;
#9132 = DIRECTION ( 'NONE',  ( 0.2306359803922031215, 0.9730401042858033422, -1.407521210652540462E-17 ) ) ;
#9133 = DATE_TIME_ROLE ( 'creation_date' ) ;
#9134 = MANIFOLD_SOLID_BREP ( 'Imported1', #8306 ) ;
#9135 = PLANE ( 'NONE',  #8965 ) ;
#9136 = COORDINATED_UNIVERSAL_TIME_OFFSET ( 0, 0, .AHEAD. ) ;
#9137 = LINE ( 'NONE', #15827, #20389 ) ;
#9138 = LOCAL_TIME ( 14, 11, 27.00000000000000000, #10698 ) ;
#9139 = LOCAL_TIME ( 14, 11, 27.00000000000000000, #5402 ) ;
#9140 = FACE_OUTER_BOUND ( 'NONE', #9872, .T. ) ;
#9141 = EDGE_CURVE ( 'NONE', #90, #4999, #7653, .T. ) ;
#9142 = AXIS2_PLACEMENT_3D ( 'NONE', #6140, #13394, #774 ) ;
#9143 = PERSON_AND_ORGANIZATION_ROLE ( 'design_owner' ) ;
#9144 = ORIENTED_EDGE ( 'NONE', *, *, #13435, .T. ) ;
#9145 = DIRECTION ( 'NONE',  ( -6.123230199561459225E-17, -4.868008300101910084E-15, -1.000000000000000000 ) ) ;
#9146 = CIRCLE ( 'NONE', #3833, 5.000000000000004441 ) ;
#9147 = ORIENTED_EDGE ( 'NONE', *, *, #4711, .F. ) ;
#9148 = DIRECTION ( 'NONE',  ( -0.2306359803922085339, -0.9730401042858022320, 0.000000000000000000 ) ) ;
#9149 = DIRECTION ( 'NONE',  ( 2.269747459788990007E-13, 2.220446049250330436E-15, 1.000000000000000000 ) ) ;
#9150 = DIRECTION ( 'NONE',  ( -0.9730401042858035643, 0.2306359803922028717, 5.958148513035547083E-17 ) ) ;
#9151 = ORIENTED_EDGE ( 'NONE', *, *, #21731, .F. ) ;
#9152 = ORIENTED_EDGE ( 'NONE', *, *, #11334, .F. ) ;
#9153 = CARTESIAN_POINT ( 'NONE',  ( 43.45766680872420551, 21.27115113520920175, -20.00000000000000000 ) ) ;
#9154 = ORIENTED_EDGE ( 'NONE', *, *, #2872, .F. ) ;
#9155 = CALENDAR_DATE ( 2026, 31, 10 ) ;
#9156 = LOCAL_TIME ( 14, 11, 27.00000000000000000, #20346 ) ;
#9157 = VERTEX_POINT ( 'NONE', #2545 ) ;
#9158 = ORIENTED_EDGE ( 'NONE', *, *, #13259, .F. ) ;
#9159 = DIRECTION ( 'NONE',  ( 5.101515458763170175E-16, 0.000000000000000000, 1.000000000000000000 ) ) ;
#9160 = LOCAL_TIME ( 14, 11, 27.00000000000000000, #1563 ) ;
#9161 = SPHERICAL_SURFACE ( 'NONE', #22933, 15.25000000000000000 ) ;
#9162 = APPROVAL_DATE_TIME ( #16167, #21859 ) ;
#9163 = VECTOR ( 'NONE', #4145, 1000.000000000000000 ) ;
#9164 = FACE_OUTER_BOUND ( 'NONE', #11685, .T. ) ;
#9165 = CYLINDRICAL_SURFACE ( 'NONE', #9894, 5.000000000000001776 ) ;
#9166 = LOCAL_TIME ( 14, 11, 27.00000000000000000, #19330 ) ;
#9167 =( REPRESENTATION_RELATIONSHIP ('NONE','NONE', #23243, #21569 ) REPRESENTATION_RELATIONSHIP_WITH_TRANSFORMATION ( #14452 )SHAPE_REPRESENTATION_RELATIONSHIP( ) );
#9168 =( NAMED_UNIT ( * ) SI_UNIT ( $, .STERADIAN. ) SOLID_ANGLE_UNIT ( ) );
#9169 = EDGE_LOOP ( 'NONE', ( #6137, #13080 ) ) ;
#9170 = FACE_OUTER_BOUND ( 'NONE', #8606, .T. ) ;
#9171 = MANIFOLD_SOLID_BREP ( 'Imported1', #17788 ) ;
#9172 = MECHANICAL_CONTEXT ( 'NONE', #11119, 'mechanical' ) ;
#9173 = LOCAL_TIME ( 14, 11, 27.00000000000000000, #22475 ) ;
#9174 = ORIENTED_EDGE ( 'NONE', *, *, #2005, .T. ) ;
#9175 = LINE ( 'NONE', #19747, #9492 ) ;
#9176 = AXIS2_PLACEMENT_3D ( 'NONE', #8143, #13155, #2218 ) ;
#9177 = CARTESIAN_POINT ( 'NONE',  ( 36.79228697538940196, -6.849707878650439952, 3.399999999999999911 ) ) ;
#9178 = CARTESIAN_POINT ( 'NONE',  ( 31.11077410011089839, -1.335996977273150144, 15.00000000000000000 ) ) ;
#9179 = DIRECTION ( 'NONE',  ( -0.2306359803922102825, -0.9730401042858017879, 4.163336342344335449E-15 ) ) ;
#9180 = CARTESIAN_POINT ( 'NONE',  ( 96.81657767996070163, -18.09668638014640152, 13.00000000000000000 ) ) ;
#9181 = ORIENTED_EDGE ( 'NONE', *, *, #18606, .T. ) ;
#9182 = VERTEX_POINT ( 'NONE', #14799 ) ;
#9183 = CARTESIAN_POINT ( 'NONE',  ( 33.90629338714457930, 8.574134987387148854, 8.864716985163932250 ) ) ;
#9184 = UNCERTAINTY_MEASURE_WITH_UNIT (LENGTH_MEASURE( 1.000000000000000082E-05 ), #23203, 'distance_accuracy_value', 'NONE');
#9185 = EDGE_CURVE ( 'NONE', #14619, #23452, #14894, .T. ) ;
#9186 = EDGE_CURVE ( 'NONE', #10599, #23068, #9918, .T. ) ;
#9187 = ORIENTED_EDGE ( 'NONE', *, *, #13271, .T. ) ;
#9188 = DIRECTION ( 'NONE',  ( -0.9730401042858022320, 0.2306359803922080343, 5.959266323858941219E-17 ) ) ;
#9189 = CARTESIAN_POINT ( 'NONE',  ( -17.50000000397459843, 22.95208920922877738, -7.999999999996137312 ) ) ;
#9190 = ORIENTED_EDGE ( 'NONE', *, *, #10887, .F. ) ;
#9191 = CARTESIAN_POINT ( 'NONE',  ( 28.14554285793940025, -3.006546890859610244, -11.00000000000039968 ) ) ;
#9192 = ORIENTED_EDGE ( 'NONE', *, *, #4262, .F. ) ;
#9193 = LOCAL_TIME ( 14, 11, 27.00000000000000000, #14160 ) ;
#9194 = CARTESIAN_POINT ( 'NONE',  ( 63.86158900585790832, 8.213232408304291354, 1.054077144304177195E-14 ) ) ;
#9195 = PERSON_AND_ORGANIZATION_ROLE ( 'creator' ) ;
#9196 = CARTESIAN_POINT ( 'NONE',  ( -1.262685242559879909E-14, -17.30000000000000071, 2.500000000000000000 ) ) ;
#9197 = ADVANCED_FACE ( 'NONE', ( #17149, #20358 ), #20253, .F. ) ;
#9198 = CIRCLE ( 'NONE', #6940, 2.500000000000000444 ) ;
#9199 = LOCAL_TIME ( 14, 11, 27.00000000000000000, #22731 ) ;
#9200 = DIRECTION ( 'NONE',  ( -0.9730401042858036753, 0.2306359803922031493, -2.740969466505752002E-16 ) ) ;
#9201 = AXIS2_PLACEMENT_3D ( 'NONE', #4316, #18453, #22113 ) ;
#9202 = CARTESIAN_POINT ( 'NONE',  ( 32.57408586390383221, 18.71231041770096226, 12.99999999999979927 ) ) ;
#9203 = CARTESIAN_POINT ( 'NONE',  ( 0.000000000000000000, 0.000000000000000000, 0.000000000000000000 ) ) ;
#9204 = DIRECTION ( 'NONE',  ( -1.187319687680494078E-16, -2.805478249478265308E-20, -1.000000000000000000 ) ) ;
#9205 = DIRECTION ( 'NONE',  ( 0.005235963827108352890, -0.9999862922474493931, -2.671135040551771006E-18 ) ) ;
#9206 = CARTESIAN_POINT ( 'NONE',  ( 37.40573311221180575, -6.139030851290243618, -13.00000000000000000 ) ) ;
#9207 = DESIGN_CONTEXT ( 'detailed design', #1867, 'design' ) ;
#9208 = CC_DESIGN_SECURITY_CLASSIFICATION ( #7318, ( #15652 ) ) ;
#9209 = FACE_OUTER_BOUND ( 'NONE', #955, .T. ) ;
#9210 = DIRECTION ( 'NONE',  ( -0.9730401042858036753, 0.2306359803922028995, 5.959266323858677443E-17 ) ) ;
#9211 = VECTOR ( 'NONE', #221, 1000.000000000000114 ) ;
#9212 = CARTESIAN_POINT ( 'NONE',  ( -0.5391976746782148888, 18.33937061236850141, 3.301631463538509622E-17 ) ) ;
#9213 = ORIENTED_EDGE ( 'NONE', *, *, #2134, .F. ) ;
#9214 = EDGE_CURVE ( 'NONE', #1171, #7380, #18374, .T. ) ;
#9215 = MANIFOLD_SOLID_BREP ( 'Imported1', #18556 ) ;
#9216 = AXIS2_PLACEMENT_3D ( 'NONE', #20023, #22146, #3746 ) ;
#9217 = ORIENTED_EDGE ( 'NONE', *, *, #1040, .T. ) ;
#9218 = DIRECTION ( 'NONE',  ( -0.9999862922464843873, -0.005235964011423952132, -1.932211830181250652E-17 ) ) ;
#9219 = LINE ( 'NONE', #21794, #10606 ) ;
#9220 = ORIENTED_EDGE ( 'NONE', *, *, #7641, .F. ) ;
#9221 = CC_DESIGN_DATE_AND_TIME_ASSIGNMENT ( #15472, #11948, ( #6423 ) ) ;
#9222 = PLANE ( 'NONE',  #20959 ) ;
#9223 = ORIENTED_EDGE ( 'NONE', *, *, #21420, .F. ) ;
#9224 = APPROVAL ( #6188, 'UNSPECIFIED' ) ;
#9225 = CARTESIAN_POINT ( 'NONE',  ( -20.00000000397270128, 22.95208919257159863, 5.500000000004459544 ) ) ;
#9226 = AXIS2_PLACEMENT_3D ( 'NONE', #15005, #2433, #13352 ) ;
#9227 = CALENDAR_DATE ( 2026, 31, 10 ) ;
#9228 = CARTESIAN_POINT ( 'NONE',  ( 36.07092311366589854, 11.78608357701213905, -8.759424124907058129 ) ) ;
#9229 = AXIS2_PLACEMENT_3D ( 'NONE', #7479, #18528, #9029 ) ;
#9230 = EDGE_CURVE ( 'NONE', #747, #13595, #4206, .T. ) ;
#9231 = EDGE_CURVE ( 'NONE', #9101, #18682, #15328, .T. ) ;
#9232 = LOCAL_TIME ( 14, 11, 27.00000000000000000, #19078 ) ;
#9233 = CALENDAR_DATE ( 2026, 31, 10 ) ;
#9234 = PLANE ( 'NONE',  #14998 ) ;
#9235 = AXIS2_PLACEMENT_3D ( 'NONE', #5243, #14384, #13058 ) ;
#9236 = ORIENTED_EDGE ( 'NONE', *, *, #15383, .T. ) ;
#9237 = VECTOR ( 'NONE', #1555, 1000.000000000000000 ) ;
#9238 = CARTESIAN_POINT ( 'NONE',  ( 2.664535259100379799E-14, -1.554450629062440126E-15, 5.000000000000000000 ) ) ;
#9239 = ORIENTED_EDGE ( 'NONE', *, *, #1084, .T. ) ;
#9240 = DIRECTION ( 'NONE',  ( 0.9730401042858035643, -0.2306359803922028717, 2.740969466505749044E-16 ) ) ;
#9241 = VERTEX_POINT ( 'NONE', #15010 ) ;
#9242 = CIRCLE ( 'NONE', #22510, 2.500000000000000888 ) ;
#9243 = DIRECTION ( 'NONE',  ( 0.9730401042858035643, -0.2306359803922028717, -5.432877459303547053E-17 ) ) ;
#9244 = DIRECTION ( 'NONE',  ( -0.9730401042858035643, 0.2306359803922028717, 5.958148513035547083E-17 ) ) ;
#9245 = CARTESIAN_POINT ( 'NONE',  ( -20.00000000397270128, 22.95208919257159863, 5.000000000004460432 ) ) ;
#9246 = ORIENTED_EDGE ( 'NONE', *, *, #6669, .F. ) ;
#9247 = ADVANCED_FACE ( 'NONE', ( #17023 ), #906, .F. ) ;
#9248 = VECTOR ( 'NONE', #9951, 1000.000000000000227 ) ;
#9249 = ITEM_DEFINED_TRANSFORMATION ( 'NONE', 'NONE', #22363,  #12739 ) ;
#9250 = CARTESIAN_POINT ( 'NONE',  ( -14.00000000202540029, 1.899127378930369980, 5.500000000004440004 ) ) ;
#9251 = CIRCLE ( 'NONE', #7001, 4.750000000000000000 ) ;
#9252 = ORIENTED_EDGE ( 'NONE', *, *, #18675, .T. ) ;
#9254 = DATE_TIME_ROLE ( 'classification_date' ) ;
#9253 = CC_DESIGN_DATE_AND_TIME_ASSIGNMENT ( #12348, #17560, ( #17062 ) ) ;
#9255 = ORIENTED_EDGE ( 'NONE', *, *, #19640, .T. ) ;
#9256 = EDGE_LOOP ( 'NONE', ( #15488, #18036, #20908, #19383, #14472, #4714 ) ) ;
#9257 = CC_DESIGN_PERSON_AND_ORGANIZATION_ASSIGNMENT ( #22200, #5939, ( #23156 ) ) ;
#9258 = DIRECTION ( 'NONE',  ( -0.9579954394086668268, -0.2867834340965239592, 1.485305508172449974E-15 ) ) ;
#9259 = PERSON_AND_ORGANIZATION ( #11966, #8758 ) ;
#9260 = EDGE_CURVE ( 'NONE', #1739, #1462, #3972, .T. ) ;
#9261 = ADVANCED_FACE ( 'NONE', ( #15721 ), #17077, .F. ) ;
#9262 = DIRECTION ( 'NONE',  ( -1.000000000000000000, 0.000000000000000000, 0.000000000000000000 ) ) ;
#9263 = APPROVAL_DATE_TIME ( #11051, #10254 ) ;
#9264 = DIRECTION ( 'NONE',  ( -1.000000000000000000, 0.000000000000000000, 0.000000000000000000 ) ) ;
#9265 = AXIS2_PLACEMENT_3D ( 'NONE', #18115, #16318, #14554 ) ;
#9266 = DIRECTION ( 'NONE',  ( 0.005235963827121942714, -0.9999862922474493931, -2.738609489598291197E-14 ) ) ;
#9267 = PERSON_AND_ORGANIZATION_ROLE ( 'design_owner' ) ;
#9268 = ORIENTED_EDGE ( 'NONE', *, *, #23114, .F. ) ;
#9269 = CARTESIAN_POINT ( 'NONE',  ( -60.02994014102380049, 8.478793778983318319, -5.000000000000000000 ) ) ;
#9270 = ORIENTED_EDGE ( 'NONE', *, *, #12055, .F. ) ;
#9271 = EDGE_CURVE ( 'NONE', #22078, #12251, #18604, .T. ) ;
#9272 = FACE_OUTER_BOUND ( 'NONE', #2737, .T. ) ;
#9273 = CARTESIAN_POINT ( 'NONE',  ( 36.89121352362745654, 22.27682603178741161, 15.00000000000000178 ) ) ;
#9274 = CARTESIAN_POINT ( 'NONE',  ( -67.31243952378076756, 7.647659333759914801, 1.570137360108866347E-15 ) ) ;
#9275 = ORIENTED_EDGE ( 'NONE', *, *, #709, .T. ) ;
#9276 = ORIENTED_EDGE ( 'NONE', *, *, #14448, .T. ) ;
#9277 = CARTESIAN_POINT ( 'NONE',  ( 5.750000000000139444, -20.33108891324529921, -2.500000000000000000 ) ) ;
#9278 = EDGE_LOOP ( 'NONE', ( #20192, #3649, #23424, #15052 ) ) ;
#9279 = APPROVAL_STATUS ( 'not_yet_approved' ) ;
#9280 = ADVANCED_FACE ( 'NONE', ( #6588 ), #19058, .F. ) ;
#9281 = ORIENTED_EDGE ( 'NONE', *, *, #16572, .T. ) ;
#9282 = ORIENTED_EDGE ( 'NONE', *, *, #1057, .T. ) ;
#9283 = LINE ( 'NONE', #10850, #13047 ) ;
#9284 = DIRECTION ( 'NONE',  ( 3.099353312215989243E-62, -1.534091707905539548E-92, -1.000000000000000000 ) ) ;
#9285 = PERSON_AND_ORGANIZATION ( #11966, #8758 ) ;
#9286 = EDGE_CURVE ( 'NONE', #747, #8538, #17743, .T. ) ;
#9287 = CARTESIAN_POINT ( 'NONE',  ( 36.30836311812279860, 20.59233593730780143, -13.00000000000049916 ) ) ;
#9288 = EDGE_CURVE ( 'NONE', #16446, #21387, #363, .T. ) ;
#9289 = ORIENTED_EDGE ( 'NONE', *, *, #1038, .T. ) ;
#9290 = DIRECTION ( 'NONE',  ( -0.2306359803922033436, -0.9730401042858034533, 0.000000000000000000 ) ) ;
#9291 = MANIFOLD_SOLID_BREP ( 'Imported1', #7546 ) ;
#9292 = PERSON_AND_ORGANIZATION_ROLE ( 'design_supplier' ) ;
#9293 = VECTOR ( 'NONE', #13518, 1000.000000000000000 ) ;
#9294 = ORIENTED_EDGE ( 'NONE', *, *, #18695, .F. ) ;
#9295 = DIRECTION ( 'NONE',  ( -0.9730401042858036753, 0.2306359803922028995, 5.959266323858677443E-17 ) ) ;
#9296 = FACE_OUTER_BOUND ( 'NONE', #18402, .T. ) ;
#9297 = DIRECTION ( 'NONE',  ( 0.9730401042858035643, -0.2306359803922024276, 0.000000000000000000 ) ) ;
#9298 = CARTESIAN_POINT ( 'NONE',  ( -22.50000000000149925, -20.00000001665528160, -6.749999999994902744 ) ) ;
#9299 = CARTESIAN_POINT ( 'NONE',  ( -30.15694676875160241, 9.287188980624568657, 3.750000000000000000 ) ) ;
#9300 = EDGE_LOOP ( 'NONE', ( #459, #10409, #17061, #12499, #17426 ) ) ;
#9301 = CARTESIAN_POINT ( 'NONE',  ( 35.11747397072458199, 7.763535785894707608, 8.759424124906642461 ) ) ;
#9302 = CC_DESIGN_PERSON_AND_ORGANIZATION_ASSIGNMENT ( #9564, #16792, ( #8384 ) ) ;
#9303 = PRODUCT_DEFINITION_SHAPE ( 'NONE', 'NONE',  #23501 ) ;
#9304 = VERTEX_POINT ( 'NONE', #10400 ) ;
#9305 = EDGE_LOOP ( 'NONE', ( #12694, #18622, #17887, #22963, #22256, #16365 ) ) ;
#9306 = DIRECTION ( 'NONE',  ( -9.248903203239929993E-11, 1.000000000000000000, 0.000000000000000000 ) ) ;
#9307 = CARTESIAN_POINT ( 'NONE',  ( 35.01760859121469593, 7.342209420738822878, -17.70000000000048956 ) ) ;
#9308 = ORIENTED_EDGE ( 'NONE', *, *, #19831, .F. ) ;
#9309 = DIRECTION ( 'NONE',  ( -0.2306359803922094498, -0.9730401042858020100, 1.412237191019847142E-17 ) ) ;
#9310 = ORIENTED_EDGE ( 'NONE', *, *, #21447, .T. ) ;
#9311 = AXIS2_PLACEMENT_3D ( 'NONE', #16118, #5539, #18027 ) ;
#9312 = DIRECTION ( 'NONE',  ( 2.982858504489139758E-17, -2.441916418604790135E-15, -1.000000000000000000 ) ) ;
#9313 = SHAPE_REPRESENTATION ( '1602p_c_12', ( #12739 ), #14249 ) ;
#9314 = DIRECTION ( 'NONE',  ( 0.000000000000000000, 0.000000000000000000, -1.000000000000000000 ) ) ;
#9315 =( NAMED_UNIT ( * ) SI_UNIT ( $, .STERADIAN. ) SOLID_ANGLE_UNIT ( ) );
#9316 = CARTESIAN_POINT ( 'NONE',  ( -20.00000000000000000, -22.50000000000000000, 5.000000000004565237 ) ) ;
#9317 = EDGE_CURVE ( 'NONE', #23097, #21550, #7986, .T. ) ;
#9318 = CARTESIAN_POINT ( 'NONE',  ( -30.72441677844210162, -6.660963241697129611, 2.999000000000090260 ) ) ;
#9319 = DATE_TIME_ROLE ( 'classification_date' ) ;
#9320 = LINE ( 'NONE', #21784, #7373 ) ;
#9321 = DIRECTION ( 'NONE',  ( 2.269747459788994803E-13, 2.220446049250330436E-15, 1.000000000000000000 ) ) ;
#9322 = CARTESIAN_POINT ( 'NONE',  ( 30.50389457288209982, -2.378844316418859517, -13.00000000000000000 ) ) ;
#9323 =( GEOMETRIC_REPRESENTATION_CONTEXT ( 3 ) GLOBAL_UNCERTAINTY_ASSIGNED_CONTEXT ( ( #21770 ) ) GLOBAL_UNIT_ASSIGNED_CONTEXT ( ( #6478, #4816, #19894 ) ) REPRESENTATION_CONTEXT ( 'NONE', 'WORKASPACE' ) );
#9324 = DIRECTION ( 'NONE',  ( 0.1997366180463766849, 0.8426774492125652660, -0.5000000000000004441 ) ) ;
#9325 = LINE ( 'NONE', #5524, #11922 ) ;
#9326 = CARTESIAN_POINT ( 'NONE',  ( 35.59419854219520118, 9.774809681453518806, 19.78350000000000009 ) ) ;
#9327 = ORIENTED_EDGE ( 'NONE', *, *, #5087, .F. ) ;
#9328 = AXIS2_PLACEMENT_3D ( 'NONE', #22495, #9442, #6238 ) ;
#9329 = MANIFOLD_SOLID_BREP ( 'Imported1', #15506 ) ;
#9330 = ORIENTED_EDGE ( 'NONE', *, *, #2387, .T. ) ;
#9331 = FACE_OUTER_BOUND ( 'NONE', #17216, .T. ) ;
#9332 = DIRECTION ( 'NONE',  ( 0.9730401042858036753, -0.2306359803922031493, 2.804983810440361760E-16 ) ) ;
#9333 = VERTEX_POINT ( 'NONE', #11954 ) ;
#9334 = LINE ( 'NONE', #16558, #14888 ) ;
#9335 = EDGE_LOOP ( 'NONE', ( #754, #11018, #21019, #2168, #15781, #5202, #18093, #6217, #4031 ) ) ;
#9336 = DIRECTION ( 'NONE',  ( 0.9730401042858024541, -0.2306359803922080898, -5.959266323858942451E-17 ) ) ;
#9337 = DATE_AND_TIME ( #2324, #5806 ) ;
#9338 = DIRECTION ( 'NONE',  ( -6.281952996264290168E-17, -4.969341027148640384E-15, -1.000000000000000000 ) ) ;
#9339 = SECURITY_CLASSIFICATION_LEVEL ( 'unclassified' ) ;
#9340 = CARTESIAN_POINT ( 'NONE',  ( 35.79393516024157407, 10.61748713066584671, -27.19000000000050221 ) ) ;
#9341 = ORIENTED_EDGE ( 'NONE', *, *, #16029, .F. ) ;
#9342 = AXIS2_PLACEMENT_3D ( 'NONE', #15556, #4757, #6064 ) ;
#9343 = EDGE_CURVE ( 'NONE', #19229, #20796, #17274, .T. ) ;
#9344 = LINE ( 'NONE', #299, #8869 ) ;
#9345 = ORIENTED_EDGE ( 'NONE', *, *, #6017, .T. ) ;
#9346 = CARTESIAN_POINT ( 'NONE',  ( -62.93867965702761325, 12.67062903583649991, 3.427095671567209849E-15 ) ) ;
#9347 = CC_DESIGN_PERSON_AND_ORGANIZATION_ASSIGNMENT ( #13507, #9839, ( #17915 ) ) ;
#9348 = ORIENTED_EDGE ( 'NONE', *, *, #20530, .T. ) ;
#9349 = CYLINDRICAL_SURFACE ( 'NONE', #22993, 3.499999999999999556 ) ;
#9350 = DIRECTION ( 'NONE',  ( 1.000000000000000000, 0.000000000000000000, 0.000000000000000000 ) ) ;
#9351 = CYLINDRICAL_SURFACE ( 'NONE', #10302, 2.500000000000000000 ) ;
#9352 = ORIENTED_EDGE ( 'NONE', *, *, #4250, .F. ) ;
#9353 = EDGE_CURVE ( 'NONE', #20776, #3781, #3318, .T. ) ;
#9354 = EDGE_CURVE ( 'NONE', #2378, #9721, #23131, .T. ) ;
#9355 = VECTOR ( 'NONE', #22090, 1000.000000000000000 ) ;
#9356 = CALENDAR_DATE ( 2026, 31, 10 ) ;
#9357 = VECTOR ( 'NONE', #3706, 1000.000000000000000 ) ;
#9358 = CARTESIAN_POINT ( 'NONE',  ( 30.57814311865390167, -3.583136841839989817, 15.00000000000000000 ) ) ;
#9359 = VECTOR ( 'NONE', #871, 1000.000000000000114 ) ;
#9360 = VERTEX_POINT ( 'NONE', #10508 ) ;
#9361 = PERSON_AND_ORGANIZATION ( #11966, #8758 ) ;
#9362 = DIRECTION ( 'NONE',  ( 2.979611953927833651E-09, -0.4472135954999619800, 0.8944271909999139680 ) ) ;
#9363 = VERTEX_POINT ( 'NONE', #1449 ) ;
#9364 = ORIENTED_EDGE ( 'NONE', *, *, #22486, .F. ) ;
#9365 = DIRECTION ( 'NONE',  ( -2.982858504577319616E-17, 2.441916418604790135E-15, 1.000000000000000000 ) ) ;
#9366 = PERSON_AND_ORGANIZATION ( #11966, #8758 ) ;
#9367 = MANIFOLD_SOLID_BREP ( 'Imported1', #22698 ) ;
#9368 = CARTESIAN_POINT ( 'NONE',  ( 36.82688237244705221, -6.703751863008963419, 13.00000000000000355 ) ) ;
#9369 = COORDINATED_UNIVERSAL_TIME_OFFSET ( 0, 0, .AHEAD. ) ;
#9370 = AXIS2_PLACEMENT_3D ( 'NONE', #19522, #3245, #23182 ) ;
#9371 = FACE_OUTER_BOUND ( 'NONE', #4153, .T. ) ;
#9372 = EDGE_CURVE ( 'NONE', #15812, #22407, #11406, .T. ) ;
#9373 = AXIS2_PLACEMENT_3D ( 'NONE', #6125, #18379, #7560 ) ;
#9374 = VECTOR ( 'NONE', #14863, 1000.000000000000000 ) ;
#9375 =( NAMED_UNIT ( * ) SI_UNIT ( $, .STERADIAN. ) SOLID_ANGLE_UNIT ( ) );
#9376 = CARTESIAN_POINT ( 'NONE',  ( -12.57176879866004349, 20.12926994965922134, -3.157842470436450709E-15 ) ) ;
#9377 = PRODUCT_DEFINITION ( 'UNKNOWN', '', #17948, #18010 ) ;
#9378 = COORDINATED_UNIVERSAL_TIME_OFFSET ( 0, 0, .AHEAD. ) ;
#9379 = APPROVAL ( #3426, 'UNSPECIFIED' ) ;
#9380 = ORIENTED_EDGE ( 'NONE', *, *, #5345, .T. ) ;
#9381 = FACE_OUTER_BOUND ( 'NONE', #16692, .T. ) ;
#9382 = ORIENTED_EDGE ( 'NONE', *, *, #2394, .F. ) ;
#9383 = ADVANCED_FACE ( 'NONE', ( #16071 ), #23413, .F. ) ;
#9384 = EDGE_CURVE ( 'NONE', #8174, #18157, #7170, .T. ) ;
#9385 = LINE ( 'NONE', #4277, #1026 ) ;
#9386 = PRODUCT_DEFINITION ( 'UNKNOWN', '', #20866, #6623 ) ;
#9387 = LINE ( 'NONE', #12724, #896 ) ;
#9388 = DIRECTION ( 'NONE',  ( 0.2306359803922033713, 0.9730401042858035643, -4.741332172907925165E-18 ) ) ;
#9389 = AXIS2_PLACEMENT_3D ( 'NONE', #2758, #19262, #8333 ) ;
#9390 = ORIENTED_EDGE ( 'NONE', *, *, #2389, .T. ) ;
#9391 = ORIENTED_EDGE ( 'NONE', *, *, #17007, .F. ) ;
#9392 = DIRECTION ( 'NONE',  ( -0.9730401042858035643, 0.2306359803922028717, 6.126766849694256332E-17 ) ) ;
#9393 = ORIENTED_EDGE ( 'NONE', *, *, #19192, .F. ) ;
#9394 = APPROVAL_STATUS ( 'not_yet_approved' ) ;
#9395 = VECTOR ( 'NONE', #21441, 1000.000000000000114 ) ;
#9396 = AXIS2_PLACEMENT_3D ( 'NONE', #20243, #14768, #16651 ) ;
#9397 = ORIENTED_EDGE ( 'NONE', *, *, #16655, .F. ) ;
#9398 = VERTEX_POINT ( 'NONE', #21759 ) ;
#9399 = CARTESIAN_POINT ( 'NONE',  ( 43.84419854219520829, -33.09999999999998721, 25.00000000000000000 ) ) ;
#9400 = CIRCLE ( 'NONE', #22259, 2.066999999999999726 ) ;
#9401 = CARTESIAN_POINT ( 'NONE',  ( -19.49999999982379961, -0.1021026942259700004, -2.500000000000090150 ) ) ;
#9402 = PERSON_AND_ORGANIZATION ( #11966, #8758 ) ;
#9403 = LINE ( 'NONE', #18794, #2144 ) ;
#9404 = CARTESIAN_POINT ( 'NONE',  ( -19.49999999982360066, -0.1021026942259700004, -1.101737663870589950E-14 ) ) ;
#9405 = AXIS2_PLACEMENT_3D ( 'NONE', #23233, #17897, #11019 ) ;
#9406 = EDGE_CURVE ( 'NONE', #10807, #935, #16289, .T. ) ;
#9407 = CONICAL_SURFACE ( 'NONE', #18906, 2.283500000000000529, 0.7853981633974476129 ) ;
#9408 = ORIENTED_EDGE ( 'NONE', *, *, #19414, .T. ) ;
#9410 = CARTESIAN_POINT ( 'NONE',  ( 38.09538026460411686, -1.352031289437131356, -12.99999999999999645 ) ) ;
#9409 = AXIS2_PLACEMENT_3D ( 'NONE', #2657, #393, #5751 ) ;
#9411 = APPROVAL_STATUS ( 'not_yet_approved' ) ;
#9412 = EDGE_CURVE ( 'NONE', #171, #10848, #14276, .T. ) ;
#9413 = CONICAL_SURFACE ( 'NONE', #284, 1.033500000000000529, 1.029744258676650093 ) ;
#9414 = ORIENTED_EDGE ( 'NONE', *, *, #22775, .T. ) ;
#9415 = DIRECTION ( 'NONE',  ( -0.4865200521429014491, 0.1153179901961012555, 0.8660254037844388186 ) ) ;
#9416 = DIRECTION ( 'NONE',  ( -0.9730401042858036753, 0.2306359803922028995, -2.804983810440358801E-16 ) ) ;
#9417 = EDGE_CURVE ( 'NONE', #12312, #20142, #5494, .T. ) ;
#9418 = CARTESIAN_POINT ( 'NONE',  ( -20.00000000000000000, -20.00000000000000000, 0.000000000000000000 ) ) ;
#9419 = DIRECTION ( 'NONE',  ( -0.9730401042858024541, 0.2306359803922080898, 5.959266323858942451E-17 ) ) ;
#9420 = ADVANCED_FACE ( 'NONE', ( #10 ), #1799, .T. ) ;
#9421 = LINE ( 'NONE', #4418, #15655 ) ;
#9422 = ORIENTED_EDGE ( 'NONE', *, *, #8807, .T. ) ;
#9423 = FACE_OUTER_BOUND ( 'NONE', #12115, .T. ) ;
#9424 = DESIGN_CONTEXT ( 'detailed design', #4269, 'design' ) ;
#9425 = ORIENTED_EDGE ( 'NONE', *, *, #12716, .T. ) ;
#9426 = VERTEX_POINT ( 'NONE', #7404 ) ;
#9427 = DIRECTION ( 'NONE',  ( 4.028143194477080210E-16, 2.054129435991050111E-15, 1.000000000000000000 ) ) ;
#9428 = DIRECTION ( 'NONE',  ( -0.9730401042858036753, 0.2306359803922031493, 5.432877459303543355E-17 ) ) ;
#9429 = AXIS2_PLACEMENT_3D ( 'NONE', #6367, #11975, #21195 ) ;
#9430 = VERTEX_POINT ( 'NONE', #10977 ) ;
#9431 = LINE ( 'NONE', #14882, #18348 ) ;
#9432 = DIRECTION ( 'NONE',  ( 5.899155740360661039E-30, 4.861311874477930828E-15, 1.000000000000000000 ) ) ;
#9433 = CIRCLE ( 'NONE', #2210, 4.250000000000000000 ) ;
#9434 = APPROVAL_STATUS ( 'not_yet_approved' ) ;
#9435 = FACE_OUTER_BOUND ( 'NONE', #9035, .T. ) ;
#9436 = CARTESIAN_POINT ( 'NONE',  ( 61.45890873801150178, 17.00438549795330090, -13.00000000000000000 ) ) ;
#9437 = PLANE ( 'NONE',  #1798 ) ;
#9438 = CALENDAR_DATE ( 2026, 31, 10 ) ;
#9439 = EDGE_CURVE ( 'NONE', #19340, #7141, #12746, .T. ) ;
#9440 = DIRECTION ( 'NONE',  ( 2.269747459789000104E-13, 2.220446049250330436E-15, 1.000000000000000000 ) ) ;
#9441 = DIRECTION ( 'NONE',  ( 0.2306359803922095053, 0.9730401042858018990, 0.000000000000000000 ) ) ;
#9442 = DIRECTION ( 'NONE',  ( 0.000000000000000000, 1.000000000000000000, 0.000000000000000000 ) ) ;
#9443 = LINE ( 'NONE', #277, #11062 ) ;
#9444 = CLOSED_SHELL ( 'NONE', ( #9922, #9632, #14478, #14279, #11038, #7823, #10827, #15591, #13447, #19048, #3838, #1974, #3423, #11917, #21979, #7094, #13997, #17089, #18931, #21284, #6288, #19107, #12311, #6225, #17819, #1134, #1571, #21671, #11109, #18047, #6163, #2472, #6314, #2453, #7504, #16699, #4932, #2517, #8990, #16441 ) ) ;
#9445 = CARTESIAN_POINT ( 'NONE',  ( 28.89837840081079889, -1.998294948772169954, 13.00000000000019895 ) ) ;
#9446 = FACE_OUTER_BOUND ( 'NONE', #7378, .T. ) ;
#9447 = ORIENTED_EDGE ( 'NONE', *, *, #555, .F. ) ;
#9448 = MANIFOLD_SOLID_BREP ( 'Imported1', #4502 ) ;
#9449 = ORIENTED_EDGE ( 'NONE', *, *, #13917, .F. ) ;
#9450 = CARTESIAN_POINT ( 'NONE',  ( -31.64160538070510142, 6.334412527122579739, -2.500000000000000000 ) ) ;
#9451 = SHAPE_REPRESENTATION ( '1602p_c_13', ( #12739 ), #16529 ) ;
#9452 = DIRECTION ( 'NONE',  ( 9.912705577010324563E-16, 2.478176394252581338E-15, -1.000000000000000000 ) ) ;
#9453 = ORIENTED_EDGE ( 'NONE', *, *, #10159, .F. ) ;
#9454 = CIRCLE ( 'NONE', #17792, 2.499999999999998668 ) ;
#9455 = FACE_OUTER_BOUND ( 'NONE', #22455, .T. ) ;
#9456 = ADVANCED_FACE ( 'NONE', ( #18328 ), #19980, .F. ) ;
#9457 = EDGE_LOOP ( 'NONE', ( #21075, #11644, #76, #6880 ) ) ;
#9458 = DIRECTION ( 'NONE',  ( -0.2306359803922085339, -0.9730401042858022320, 0.000000000000000000 ) ) ;
#9459 = COORDINATED_UNIVERSAL_TIME_OFFSET ( 0, 0, .AHEAD. ) ;
#9460 = DIRECTION ( 'NONE',  ( 0.000000000000000000, -1.000000000000000000, 0.000000000000000000 ) ) ;
#9461 = APPROVAL_STATUS ( 'not_yet_approved' ) ;
#9462 = CARTESIAN_POINT ( 'NONE',  ( -26.99999999999959854, -33.09999999999999432, -25.00000000000000000 ) ) ;
#9463 = ORIENTED_EDGE ( 'NONE', *, *, #11639, .T. ) ;
#9464 = CC_DESIGN_SECURITY_CLASSIFICATION ( #11759, ( #23482 ) ) ;
#9465 = LINE ( 'NONE', #23350, #19487 ) ;
#9466 = AXIS2_PLACEMENT_3D ( 'NONE', #17864, #8505, #19185 ) ;
#9467 = ORIENTED_EDGE ( 'NONE', *, *, #14220, .F. ) ;
#9468 = DIRECTION ( 'NONE',  ( 6.281952996264339472E-17, 4.969341027148640384E-15, 1.000000000000000000 ) ) ;
#9469 = CYLINDRICAL_SURFACE ( 'NONE', #18620, 2.066999999999998394 ) ;
#9470 = ORIENTED_EDGE ( 'NONE', *, *, #9028, .F. ) ;
#9471 = CARTESIAN_POINT ( 'NONE',  ( 37.10730959030829723, 23.96304573415820016, 15.00000000000000000 ) ) ;
#9472 = CARTESIAN_POINT ( 'NONE',  ( -14.10640258711669937, 21.82649101058139962, 3.749999999999949818 ) ) ;
#9473 = FACE_OUTER_BOUND ( 'NONE', #5807, .T. ) ;
#9474 = VERTEX_POINT ( 'NONE', #12514 ) ;
#9475 = APPROVAL_STATUS ( 'not_yet_approved' ) ;
#9476 = CARTESIAN_POINT ( 'NONE',  ( 33.27705887009690144, -3.036156860537075453, 17.25000000000019895 ) ) ;
#9477 = ORIENTED_EDGE ( 'NONE', *, *, #6070, .T. ) ;
#9478 = EDGE_CURVE ( 'NONE', #2422, #9929, #9175, .T. ) ;
#9479 = CALENDAR_DATE ( 2026, 31, 10 ) ;
#9480 = CARTESIAN_POINT ( 'NONE',  ( -19.99999998648272737, 20.32708919256900160, 8.250000000004465761 ) ) ;
#9481 = ADVANCED_FACE ( 'NONE', ( #21867 ), #12909, .T. ) ;
#9482 = ORIENTED_EDGE ( 'NONE', *, *, #12716, .F. ) ;
#9483 = ORIENTED_EDGE ( 'NONE', *, *, #11180, .F. ) ;
#9484 = DIRECTION ( 'NONE',  ( -0.9080618652410672453, 0.4188360644630710894, -1.049848863090360721E-15 ) ) ;
#9485 = CONICAL_SURFACE ( 'NONE', #8349, 1.154700538379250796, 1.047197551196598297 ) ;
#9486 = AXIS2_PLACEMENT_3D ( 'NONE', #7856, #4169, #14975 ) ;
#9487 = CALENDAR_DATE ( 2026, 31, 10 ) ;
#9488 = VECTOR ( 'NONE', #20068, 1000.000000000000000 ) ;
#9489 = MANIFOLD_SOLID_BREP ( 'Imported1', #23154 ) ;
#9490 = COORDINATED_UNIVERSAL_TIME_OFFSET ( 0, 0, .AHEAD. ) ;
#9491 = CARTESIAN_POINT ( 'NONE',  ( -16.50000000144870071, -4.350228928667009498, -5.499999999996299849 ) ) ;
#9492 = VECTOR ( 'NONE', #10868, 1000.000000000000227 ) ;
#9493 = EDGE_CURVE ( 'NONE', #483, #23152, #5253, .T. ) ;
#9494 = EDGE_CURVE ( 'NONE', #13130, #10377, #3474, .T. ) ;
#9495 = CARTESIAN_POINT ( 'NONE',  ( -62.93704341833160498, 12.35813331950920002, 3.344713564077609812E-15 ) ) ;
#9496 = PERSON_AND_ORGANIZATION_ROLE ( 'design_supplier' ) ;
#9497 = PRODUCT_DEFINITION_SHAPE ( 'NONE', 'NONE',  #23502 ) ;
#9498 = CC_DESIGN_APPROVAL ( #6205, ( #9941 ) ) ;
#9499 = ORIENTED_EDGE ( 'NONE', *, *, #7190, .T. ) ;
#9500 = CYLINDRICAL_SURFACE ( 'NONE', #2718, 2.066999999999999726 ) ;
#9501 = ORIENTED_EDGE ( 'NONE', *, *, #22676, .T. ) ;
#9502 = CIRCLE ( 'NONE', #8369, 2.500000000000000000 ) ;
#9503 = CARTESIAN_POINT ( 'NONE',  ( -23.49917714535037661, 22.87619892134627975, -5.000000000000000000 ) ) ;
#9504 = CARTESIAN_POINT ( 'NONE',  ( 118.6002496876800052, -6.405594307115060282, 15.90000000000000036 ) ) ;
#9505 = DIRECTION ( 'NONE',  ( 8.911056267098788616E-18, 1.998401444326210262E-15, 1.000000000000000000 ) ) ;
#9506 = ORIENTED_EDGE ( 'NONE', *, *, #9977, .F. ) ;
#9507 = VERTEX_POINT ( 'NONE', #5606 ) ;
#9508 = DIRECTION ( 'NONE',  ( 1.224646799147353207E-16, 1.000000000000000000, -0.000000000000000000 ) ) ;
#9509 = ORIENTED_EDGE ( 'NONE', *, *, #192, .F. ) ;
#9510 = VECTOR ( 'NONE', #20503, 1000.000000000000227 ) ;
#9511 = COORDINATED_UNIVERSAL_TIME_OFFSET ( 0, 0, .AHEAD. ) ;
#9512 = EDGE_CURVE ( 'NONE', #9733, #4472, #12851, .T. ) ;
#9513 = ORIENTED_EDGE ( 'NONE', *, *, #23113, .T. ) ;
#9514 = VERTEX_POINT ( 'NONE', #21411 ) ;
#9515 = CARTESIAN_POINT ( 'NONE',  ( -1.041857140317370201, 16.21867887107140049, -4.500000000000000000 ) ) ;
#9516 = CIRCLE ( 'NONE', #10664, 3.500000000000000444 ) ;
#9517 = CARTESIAN_POINT ( 'NONE',  ( -20.00000000000000000, -20.00000000000000000, 2.500000000000000000 ) ) ;
#9518 = APPROVAL_ROLE ( '' ) ;
#9519 = PLANE ( 'NONE',  #11653 ) ;
#9520 = CC_DESIGN_DATE_AND_TIME_ASSIGNMENT ( #11756, #11539, ( #10620 ) ) ;
#9521 = CC_DESIGN_APPROVAL ( #6938, ( #14812 ) ) ;
#9522 = CC_DESIGN_PERSON_AND_ORGANIZATION_ASSIGNMENT ( #14995, #18701, ( #6135 ) ) ;
#9523 = CARTESIAN_POINT ( 'NONE',  ( -19.99999998251005806, -22.62500000000000000, 8.250000000004556355 ) ) ;
#9524 = LOCAL_TIME ( 14, 11, 27.00000000000000000, #6232 ) ;
#9525 = EDGE_CURVE ( 'NONE', #17339, #11032, #18985, .T. ) ;
#9526 = EDGE_CURVE ( 'NONE', #3206, #7204, #21244, .T. ) ;
#9527 = VECTOR ( 'NONE', #11984, 1000.000000000000114 ) ;
#9528 = VECTOR ( 'NONE', #21660, 1000.000000000000000 ) ;
#9529 = ORIENTED_EDGE ( 'NONE', *, *, #22715, .F. ) ;
#9530 = LINE ( 'NONE', #5710, #7902 ) ;
#9531 = MANIFOLD_SOLID_BREP ( 'Boss-Extrude1', #17105 ) ;
#9532 = APPROVAL_DATE_TIME ( #18799, #18154 ) ;
#9533 = EDGE_LOOP ( 'NONE', ( #399, #8849 ) ) ;
#9534 = CARTESIAN_POINT ( 'NONE',  ( 3.747449283612720006, 22.11622885388230131, -4.500000000000000000 ) ) ;
#9535 = CARTESIAN_POINT ( 'NONE',  ( 5.000000000000180300, -33.09999999999999432, -22.00000000000000000 ) ) ;
#9536 = ORIENTED_EDGE ( 'NONE', *, *, #6199, .F. ) ;
#9537 = CC_DESIGN_APPROVAL ( #9379, ( #7624 ) ) ;
#9538 = FACE_OUTER_BOUND ( 'NONE', #3585, .T. ) ;
#9539 = CARTESIAN_POINT ( 'NONE',  ( 5.000000000000000000, -27.34999999999999787, 2.500000000000000000 ) ) ;
#9540 = APPROVAL_PERSON_ORGANIZATION ( #6674, #20903, #710 ) ;
#9541 = ORIENTED_EDGE ( 'NONE', *, *, #3238, .T. ) ;
#9542 = CYLINDRICAL_SURFACE ( 'NONE', #5775, 0.3999999999999982458 ) ;
#9543 = PERSON_AND_ORGANIZATION_ROLE ( 'design_owner' ) ;
#9544 = EDGE_CURVE ( 'NONE', #17474, #9398, #1565, .T. ) ;
#9545 = ORIENTED_EDGE ( 'NONE', *, *, #8827, .F. ) ;
#9546 = LOCAL_TIME ( 14, 11, 27.00000000000000000, #13975 ) ;
#9547 = EDGE_LOOP ( 'NONE', ( #112, #13363, #15709, #20166 ) ) ;
#9548 = CYLINDRICAL_SURFACE ( 'NONE', #15278, 2.499999999999999556 ) ;
#9549 = DIRECTION ( 'NONE',  ( -0.2306359803922033436, -0.9730401042858034533, 0.000000000000000000 ) ) ;
#9550 = DIRECTION ( 'NONE',  ( -2.982858504577314686E-17, 2.441916418604790135E-15, 1.000000000000000000 ) ) ;
#9551 = ORIENTED_EDGE ( 'NONE', *, *, #16882, .T. ) ;
#9552 = APPROVAL_DATE_TIME ( #1488, #11587 ) ;
#9553 = FACE_OUTER_BOUND ( 'NONE', #4620, .T. ) ;
#9554 = CARTESIAN_POINT ( 'NONE',  ( -20.00000000000000000, -20.00000000000000000, 0.000000000000000000 ) ) ;
#9555 = ITEM_DEFINED_TRANSFORMATION ( 'NONE', 'NONE', #764,  #15545 ) ;
#9556 = FACE_OUTER_BOUND ( 'NONE', #15884, .T. ) ;
#9557 = EDGE_CURVE ( 'NONE', #134, #13843, #1688, .T. ) ;
#9558 = EDGE_CURVE ( 'NONE', #11453, #13217, #4413, .T. ) ;
#9559 = SECURITY_CLASSIFICATION ( '', '', #20991 ) ;
#9560 = VECTOR ( 'NONE', #22772, 1000.000000000000000 ) ;
#9561 = DIRECTION ( 'NONE',  ( 0.2306359803922085339, 0.9730401042858022320, 0.000000000000000000 ) ) ;
#9562 = AXIS2_PLACEMENT_3D ( 'NONE', #17486, #8472, #21051 ) ;
#9563 = CARTESIAN_POINT ( 'NONE',  ( 35.59419854219520118, 9.774809681453540122, 26.30000000000000071 ) ) ;
#9564 = PERSON_AND_ORGANIZATION ( #11966, #8758 ) ;
#9565 = CC_DESIGN_APPROVAL ( #2380, ( #19794 ) ) ;
#9566 = CARTESIAN_POINT ( 'NONE',  ( 33.87576285740830428, 21.16892588828849853, 13.00000000000000000 ) ) ;
#9567 = CARTESIAN_POINT ( 'NONE',  ( 31.14187293219668717, -1.979315439058050297, 15.00000000000011724 ) ) ;
#9568 = DIRECTION ( 'NONE',  ( 0.2306359803922029827, 0.9730401042858035643, -4.849856555169150033E-15 ) ) ;
#9569 = CARTESIAN_POINT ( 'NONE',  ( -62.91249983789198552, 7.670697574599230073, 2.731378056153440284E-17 ) ) ;
#9570 = CARTESIAN_POINT ( 'NONE',  ( -65.62876257020761273, -24.89748912807110059, 5.000000000000000000 ) ) ;
#9571 = CARTESIAN_POINT ( 'NONE',  ( -62.94070309524829554, 13.05707373847569919, -5.515665073666220062E-15 ) ) ;
#9572 = ORIENTED_EDGE ( 'NONE', *, *, #12396, .T. ) ;
#9573 = MANIFOLD_SOLID_BREP ( 'Imported1', #5262 ) ;
#9574 = EDGE_CURVE ( 'NONE', #16192, #18788, #490, .T. ) ;
#9575 = CC_DESIGN_APPROVAL ( #18376, ( #11475 ) ) ;
#9576 = ORIENTED_EDGE ( 'NONE', *, *, #13259, .T. ) ;
#9577 = DIRECTION ( 'NONE',  ( -0.5000051404512477760, 0.000000000000000000, 0.8660224359231856184 ) ) ;
#9578 = CARTESIAN_POINT ( 'NONE',  ( -29.94163891957289891, 6.343422587376370103, 3.750000000000000000 ) ) ;
#9579 = VERTEX_POINT ( 'NONE', #2271 ) ;
#9580 = VECTOR ( 'NONE', #6595, 1000.000000000000000 ) ;
#9581 = LINE ( 'NONE', #15262, #9983 ) ;
#9582 = ORIENTED_EDGE ( 'NONE', *, *, #2536, .F. ) ;
#9583 = AXIS2_PLACEMENT_3D ( 'NONE', #3523, #19562, #10448 ) ;
#9584 = AXIS2_PLACEMENT_3D ( 'NONE', #9809, #4449, #17027 ) ;
#9585 = DIRECTION ( 'NONE',  ( 0.9949874374308178560, 0.09999999677427207079, -1.179611963664228824E-14 ) ) ;
#9586 = LOCAL_TIME ( 14, 11, 27.00000000000000000, #11637 ) ;
#9587 = APPLICATION_PROTOCOL_DEFINITION ( 'international standard', 'config_control_design', 1994, #1867 ) ;
#9588 = CARTESIAN_POINT ( 'NONE',  ( 37.18843686696352790, 8.452164511700056337, -8.953813951970682083 ) ) ;
#9589 = EDGE_CURVE ( 'NONE', #15787, #15219, #8839, .T. ) ;
#9590 = AXIS2_PLACEMENT_3D ( 'NONE', #7869, #6080, #2638 ) ;
#9591 = EDGE_CURVE ( 'NONE', #13305, #11532, #602, .T. ) ;
#9592 = DATE_AND_TIME ( #16681, #21299 ) ;
#9593 = AXIS2_PLACEMENT_3D ( 'NONE', #22915, #15431, #20898 ) ;
#9594 = CARTESIAN_POINT ( 'NONE',  ( 1.836479826415680084E-19, -7.772252928343919938E-16, -8.889558542813568797E-14 ) ) ;
#9595 = ORIENTED_EDGE ( 'NONE', *, *, #20430, .F. ) ;
#9596 = LOCAL_TIME ( 14, 11, 27.00000000000000000, #10939 ) ;
#9597 = LINE ( 'NONE', #11381, #17973 ) ;
#9598 = AXIS2_PLACEMENT_3D ( 'NONE', #10841, #5235, #12831 ) ;
#9599 = EDGE_LOOP ( 'NONE', ( #7726, #16330, #13307 ) ) ;
#9600 = CYLINDRICAL_SURFACE ( 'NONE', #2976, 5.000000000000000888 ) ;
#9601 = CIRCLE ( 'NONE', #18307, 4.100000000000000533 ) ;
#9602 = VECTOR ( 'NONE', #23457, 1000.000000000000000 ) ;
#9603 = CARTESIAN_POINT ( 'NONE',  ( 114.8178196092480050, -22.36345201740219935, -13.00000000000000000 ) ) ;
#9604 = ORIENTED_EDGE ( 'NONE', *, *, #13073, .T. ) ;
#9605 = SHAPE_REPRESENTATION ( '1602p_c_16', ( #12739 ), #1734 ) ;
#9606 = LINE ( 'NONE', #4239, #18470 ) ;
#9607 = CARTESIAN_POINT ( 'NONE',  ( -19.49999999982360066, -0.1021026942259779940, -3.750000000000000000 ) ) ;
#9608 = ORIENTED_EDGE ( 'NONE', *, *, #9028, .T. ) ;
#9609 = AXIS2_PLACEMENT_3D ( 'NONE', #9571, #16803, #22246 ) ;
#9610 = CALENDAR_DATE ( 2026, 31, 10 ) ;
#9611 = DIRECTION ( 'NONE',  ( -6.662160722082822564E-09, 1.000000000000000000, -2.523234146875356491E-15 ) ) ;
#9612 = AXIS2_PLACEMENT_3D ( 'NONE', #22292, #5670, #5918 ) ;
#9613 = VERTEX_POINT ( 'NONE', #14749 ) ;
#9614 = VECTOR ( 'NONE', #15802, 999.9999999999998863 ) ;
#9615 = CC_DESIGN_PERSON_AND_ORGANIZATION_ASSIGNMENT ( #1211, #8488, ( #3463 ) ) ;
#9616 = APPROVAL_DATE_TIME ( #311, #6932 ) ;
#9617 = CARTESIAN_POINT ( 'NONE',  ( 117.1241794131703529, -12.63305097454429848, 3.419367484756719403E-14 ) ) ;
#9618 = CC_DESIGN_SECURITY_CLASSIFICATION ( #480, ( #5427 ) ) ;
#9619 = ORIENTED_EDGE ( 'NONE', *, *, #2441, .F. ) ;
#9620 = ORIENTED_EDGE ( 'NONE', *, *, #23276, .T. ) ;
#9621 = CARTESIAN_POINT ( 'NONE',  ( -20.00000000397360012, 22.95208919256889857, -3.750000000000000000 ) ) ;
#9622 = PERSON_AND_ORGANIZATION_ROLE ( 'design_supplier' ) ;
#9623 = AXIS2_PLACEMENT_3D ( 'NONE', #9756, #16857, #2244 ) ;
#9624 = VECTOR ( 'NONE', #2990, 999.9999999999998863 ) ;
#9625 = MANIFOLD_SOLID_BREP ( 'Imported1', #14742 ) ;
#9626 = CIRCLE ( 'NONE', #20219, 2.066999999999998394 ) ;
#9627 = ITEM_DEFINED_TRANSFORMATION ( 'NONE', 'NONE', #19363,  #12739 ) ;
#9628 = CARTESIAN_POINT ( 'NONE',  ( 33.27705887009690144, -3.036156860537205127, -8.750000000000399680 ) ) ;
#9629 = DIRECTION ( 'NONE',  ( 0.000000000000000000, 0.000000000000000000, 1.000000000000000000 ) ) ;
#9631 = VECTOR ( 'NONE', #5515, 1000.000000000000227 ) ;
#9630 = DIRECTION ( 'NONE',  ( 0.9730401042858035643, -0.2306359803922028717, -5.432877459303547053E-17 ) ) ;
#9632 = ADVANCED_FACE ( 'NONE', ( #15100 ), #5957, .F. ) ;
#9633 = PERSON_AND_ORGANIZATION_ROLE ( 'creator' ) ;
#9634 = CIRCLE ( 'NONE', #23108, 2.499999999999998668 ) ;
#9635 = AXIS2_PLACEMENT_3D ( 'NONE', #20732, #18617, #16826 ) ;
#9636 = ORIENTED_EDGE ( 'NONE', *, *, #10961, .F. ) ;
#9637 = APPLICATION_CONTEXT ( 'configuration controlled 3d designs of mechanical parts and assemblies' ) ;
#9638 = AXIS2_PLACEMENT_3D ( 'NONE', #16248, #3199, #17692 ) ;
#9639 = CARTESIAN_POINT ( 'NONE',  ( -20.00000000000000000, -20.00000000000000000, -4.999999999995470290 ) ) ;
#9640 = VERTEX_POINT ( 'NONE', #11683 ) ;
#9641 = DIRECTION ( 'NONE',  ( -0.005235963827108362431, 0.9999862922474493931, 5.936218956694023463E-19 ) ) ;
#9642 = AXIS2_PLACEMENT_3D ( 'NONE', #7464, #5446, #14697 ) ;
#9643 = DIRECTION ( 'NONE',  ( -2.882701132343535037E-16, -9.096985413436440085E-33, 1.000000000000000000 ) ) ;
#9644 = DIRECTION ( 'NONE',  ( -0.9730401042858035643, 0.2306359803922028717, 5.958148513035547083E-17 ) ) ;
#9645 = EDGE_LOOP ( 'NONE', ( #1855, #15293 ) ) ;
#9646 = EDGE_LOOP ( 'NONE', ( #14718, #13079, #3784, #12485, #3442 ) ) ;
#9647 = PLANE ( 'NONE',  #3771 ) ;
#9648 = VERTEX_POINT ( 'NONE', #15217 ) ;
#9649 = ADVANCED_FACE ( 'NONE', ( #6207 ), #18911, .T. ) ;
#9650 = PERSON_AND_ORGANIZATION ( #11966, #8758 ) ;
#9651 = ORIENTED_EDGE ( 'NONE', *, *, #18606, .F. ) ;
#9652 = EDGE_LOOP ( 'NONE', ( #5131, #7419, #16388, #23357 ) ) ;
#9653 = DIRECTION ( 'NONE',  ( 3.210834492181045054E-17, -2.441916418604790135E-15, -1.000000000000000000 ) ) ;
#9654 = DATE_AND_TIME ( #15204, #8808 ) ;
#9655 = DIRECTION ( 'NONE',  ( -0.9730401042858036753, 0.2306359803922031493, 5.432877459303543355E-17 ) ) ;
#9656 = VECTOR ( 'NONE', #7427, 1000.000000000000227 ) ;
#9657 = DIRECTION ( 'NONE',  ( -3.210834492181045054E-17, 2.441916418604790135E-15, 1.000000000000000000 ) ) ;
#9658 = CIRCLE ( 'NONE', #2438, 2.500000000000000888 ) ;
#9659 = ORIENTED_EDGE ( 'NONE', *, *, #11862, .T. ) ;
#9660 = DIRECTION ( 'NONE',  ( -0.9730401042858036753, 0.2306359803922031493, 5.432877459303543355E-17 ) ) ;
#9661 = ADVANCED_FACE ( 'NONE', ( #244 ), #16998, .T. ) ;
#9662 = MANIFOLD_SOLID_BREP ( 'Cut-Extrude1', #5716 ) ;
#9663 = APPLICATION_PROTOCOL_DEFINITION ( 'international standard', 'config_control_design', 1994, #13521 ) ;
#9664 = VERTEX_POINT ( 'NONE', #13215 ) ;
#9665 = DIRECTION ( 'NONE',  ( -1.000000000000000000, 0.000000000000000000, 0.000000000000000000 ) ) ;
#9666 = DIRECTION ( 'NONE',  ( 0.2306359803922028995, 0.9730401042858036753, -9.756037151021835575E-16 ) ) ;
#9667 = ORIENTED_EDGE ( 'NONE', *, *, #21584, .F. ) ;
#9668 = CC_DESIGN_PERSON_AND_ORGANIZATION_ASSIGNMENT ( #6615, #3028, ( #19794 ) ) ;
#9669 = CARTESIAN_POINT ( 'NONE',  ( 36.68971944905815974, 14.39675017681084768, -26.88000000000052481 ) ) ;
#9670 = CARTESIAN_POINT ( 'NONE',  ( 35.59419854219520118, 9.774809681453278998, -26.50000000000049738 ) ) ;
#9671 = ORIENTED_EDGE ( 'NONE', *, *, #2161, .F. ) ;
#9672 = DIRECTION ( 'NONE',  ( -0.2306359803922031770, -0.9730401042858035643, 1.407521210652529060E-17 ) ) ;
#9673 = ADVANCED_FACE ( 'NONE', ( #11219 ), #22456, .F. ) ;
#9674 = EDGE_CURVE ( 'NONE', #5643, #5737, #7861, .T. ) ;
#9675 = APPROVAL_STATUS ( 'not_yet_approved' ) ;
#9676 = VERTEX_POINT ( 'NONE', #4175 ) ;
#9677 = ORIENTED_EDGE ( 'NONE', *, *, #21118, .T. ) ;
#9678 = FACE_OUTER_BOUND ( 'NONE', #15642, .T. ) ;
#9679 = DIRECTION ( 'NONE',  ( -0.2306359803922031215, -0.9730401042858034533, 4.849856555169147667E-15 ) ) ;
#9680 = VERTEX_POINT ( 'NONE', #9775 ) ;
#9681 = APPROVAL_STATUS ( 'not_yet_approved' ) ;
#9682 = DIRECTION ( 'NONE',  ( -0.9730401042858024541, 0.2306359803922080898, 5.959266323858942451E-17 ) ) ;
#9683 = PLANE ( 'NONE',  #8251 ) ;
#9684 = CALENDAR_DATE ( 2026, 31, 10 ) ;
#9685 = CARTESIAN_POINT ( 'NONE',  ( 35.84667945578129888, -10.83917230622219918, 13.00000000000000000 ) ) ;
#9686 = ADVANCED_BREP_SHAPE_REPRESENTATION ( '', ( #9094, #12739 ), #10268 ) ;
#9687 =( LENGTH_UNIT ( ) NAMED_UNIT ( * ) SI_UNIT ( .MILLI., .METRE. ) );
#9688 = DIRECTION ( 'NONE',  ( -0.9730401042858035643, 0.2306359803922028717, -2.804983810440358308E-16 ) ) ;
#9689 = AXIS2_PLACEMENT_3D ( 'NONE', #13087, #7272, #12955 ) ;
#9690 = CARTESIAN_POINT ( 'NONE',  ( 43.45766680872420551, 21.27115113520920175, -20.00000000000000000 ) ) ;
#9691 = EDGE_CURVE ( 'NONE', #7550, #11668, #5627, .T. ) ;
#9692 = PERSON_AND_ORGANIZATION_ROLE ( 'design_supplier' ) ;
#9693 = DIRECTION ( 'NONE',  ( 0.9999862922474493931, 0.005235963827108152530, 0.000000000000000000 ) ) ;
#9694 = CARTESIAN_POINT ( 'NONE',  ( -22.99995202268966921, -0.1204285676209190525, -1.060181993030890135E-14 ) ) ;
#9695 = CC_DESIGN_DATE_AND_TIME_ASSIGNMENT ( #8912, #14477, ( #18095 ) ) ;
#9696 = CARTESIAN_POINT ( 'NONE',  ( 36.10037903421270755, -9.768828191507928693, -2.700000000000000178 ) ) ;
#9697 = CARTESIAN_POINT ( 'NONE',  ( -20.00000000397270128, 22.95208919257159863, 5.000000000004460432 ) ) ;
#9698 = CC_DESIGN_DATE_AND_TIME_ASSIGNMENT ( #9017, #87, ( #3293 ) ) ;
#9699 = DIRECTION ( 'NONE',  ( 0.005225493764075828107, -0.9999863470142589250, 2.602085213965210642E-15 ) ) ;
#9700 = CARTESIAN_POINT ( 'NONE',  ( -25.64161990512560152, 6.365892616704869944, 2.500000000000000000 ) ) ;
#9701 = EDGE_CURVE ( 'NONE', #3422, #9426, #361, .T. ) ;
#9703 = ORIENTED_EDGE ( 'NONE', *, *, #14039, .T. ) ;
#9702 = EDGE_CURVE ( 'NONE', #21424, #16270, #2155, .T. ) ;
#9704 = CIRCLE ( 'NONE', #17271, 2.499999999999999112 ) ;
#9705 = ORIENTED_EDGE ( 'NONE', *, *, #10589, .T. ) ;
#9706 = DIRECTION ( 'NONE',  ( -0.9730401042858024541, 0.2306359803922080898, 5.959266323858942451E-17 ) ) ;
#9707 = DIRECTION ( 'NONE',  ( 1.138590270679730064E-14, 2.220446049251240387E-15, 1.000000000000000000 ) ) ;
#9708 = ORIENTED_EDGE ( 'NONE', *, *, #21896, .T. ) ;
#9709 = CARTESIAN_POINT ( 'NONE',  ( 114.8178196092480050, -22.36345201740209987, 20.00000000000000000 ) ) ;
#9710 = ORIENTED_EDGE ( 'NONE', *, *, #16745, .F. ) ;
#9711 = CARTESIAN_POINT ( 'NONE',  ( -16.50000000202729922, 1.899127378699190016, -7.999999999996308730 ) ) ;
#9712 = PERSON_AND_ORGANIZATION ( #11966, #8758 ) ;
#9713 = CARTESIAN_POINT ( 'NONE',  ( 37.21329654006962784, 11.08746082399636101, -8.849422422067901195 ) ) ;
#9714 = PRODUCT_DEFINITION_SHAPE ( 'NONE', 'NONE',  #23507 ) ;
#9715 = PERSON_AND_ORGANIZATION ( #17000, #8423 ) ;
#9716 = DIRECTION ( 'NONE',  ( -0.005235963827121952255, 0.9999862922474493931, -2.738476122049126182E-14 ) ) ;
#9717 = CARTESIAN_POINT ( 'NONE',  ( 35.59419854219520118, 9.774809681453278998, -26.50000000000049738 ) ) ;
#9718 = VERTEX_POINT ( 'NONE', #16878 ) ;
#9719 = EDGE_CURVE ( 'NONE', #9304, #18306, #16632, .T. ) ;
#9720 = LINE ( 'NONE', #6256, #14921 ) ;
#9721 = VERTEX_POINT ( 'NONE', #13099 ) ;
#9722 = CARTESIAN_POINT ( 'NONE',  ( 36.82688237244700247, -6.703751863009053125, -12.99999999999999645 ) ) ;
#9723 = EDGE_CURVE ( 'NONE', #20176, #6526, #20330, .T. ) ;
#9724 = CARTESIAN_POINT ( 'NONE',  ( 38.77124482170307118, 19.70991798171191078, -13.00000000000049916 ) ) ;
#9725 = ORIENTED_EDGE ( 'NONE', *, *, #17238, .T. ) ;
#9726 = DIRECTION ( 'NONE',  ( -0.2306359803922028995, -0.9730401042858034533, 4.741332172907957521E-18 ) ) ;
#9727 = CARTESIAN_POINT ( 'NONE',  ( 35.59419854219520118, 9.774809681453330512, -17.70000000000050022 ) ) ;
#9728 = ORIENTED_EDGE ( 'NONE', *, *, #11294, .F. ) ;
#9729 = EDGE_CURVE ( 'NONE', #15201, #171, #18562, .T. ) ;
#9730 = ITEM_DEFINED_TRANSFORMATION ( 'NONE', 'NONE', #4544,  #12739 ) ;
#9731 = EDGE_CURVE ( 'NONE', #16103, #11767, #17603, .T. ) ;
#9732 = CYLINDRICAL_SURFACE ( 'NONE', #11553, 5.000000000000001776 ) ;
#9733 = VERTEX_POINT ( 'NONE', #4524 ) ;
#9734 = APPLICATION_PROTOCOL_DEFINITION ( 'international standard', 'config_control_design', 1994, #20535 ) ;
#9735 = DIRECTION ( 'NONE',  ( -3.210834492181040124E-17, 2.441916418604790135E-15, 1.000000000000000000 ) ) ;
#9736 = ORIENTED_EDGE ( 'NONE', *, *, #22553, .F. ) ;
#9737 = ORIENTED_EDGE ( 'NONE', *, *, #2603, .F. ) ;
#9738 = DIRECTION ( 'NONE',  ( -2.977235988022388482E-185, 9.605990953944227443E-124, 1.000000000000000000 ) ) ;
#9739 = APPROVAL_STATUS ( 'not_yet_approved' ) ;
#9740 = CIRCLE ( 'NONE', #2510, 2.500000000000000000 ) ;
#9741 = MANIFOLD_SOLID_BREP ( 'Cut-Extrude1', #21564 ) ;
#9742 = COORDINATED_UNIVERSAL_TIME_OFFSET ( 0, 0, .AHEAD. ) ;
#9743 = DIRECTION ( 'NONE',  ( -0.2306359803922094498, -0.9730401042858020100, 1.412237191019847142E-17 ) ) ;
#9744 =( BOUNDED_CURVE ( )  B_SPLINE_CURVE ( 2, ( #22319, #6061, #8096 ),
 .UNSPECIFIED., .F., .F. ) 
 B_SPLINE_CURVE_WITH_KNOTS ( ( 3, 3 ),
 ( 0.000000000000000000, 0.1752654207116860208 ),
 .UNSPECIFIED. ) 
 CURVE ( )  GEOMETRIC_REPRESENTATION_ITEM ( )  RATIONAL_B_SPLINE_CURVE ( ( 1.000000000000000000, 1.154700538379249908, 1.000000000000000000 ) ) 
 REPRESENTATION_ITEM ( '' )  );
#9745 = DIRECTION ( 'NONE',  ( 1.302733484953870109E-15, 5.237774525740650345E-15, 1.000000000000000000 ) ) ;
#9746 = ORIENTED_EDGE ( 'NONE', *, *, #14381, .F. ) ;
#9747 = CC_DESIGN_PERSON_AND_ORGANIZATION_ASSIGNMENT ( #12483, #4995, ( #7231 ) ) ;
#9748 = DATE_AND_TIME ( #7951, #18978 ) ;
#9749 = VECTOR ( 'NONE', #14583, 999.9999999999998863 ) ;
#9750 = CIRCLE ( 'NONE', #2528, 2.066999999999997506 ) ;
#9751 = EDGE_LOOP ( 'NONE', ( #22875, #4605, #16944, #6463, #11345 ) ) ;
#9752 = CARTESIAN_POINT ( 'NONE',  ( -62.91228861290962726, 7.630356943151859639, -4.999999999999999112 ) ) ;
#9753 = ORIENTED_EDGE ( 'NONE', *, *, #385, .T. ) ;
#9754 = DIRECTION ( 'NONE',  ( -2.269747459788994803E-13, -2.220446049250325308E-15, -1.000000000000000000 ) ) ;
#9755 = CARTESIAN_POINT ( 'NONE',  ( 37.10730959030829723, 23.96304573415810069, -15.00000000000049916 ) ) ;
#9756 = CARTESIAN_POINT ( 'NONE',  ( 28.14554285793940025, -3.006546890859610244, -11.00000000000039968 ) ) ;
#9757 = ORIENTED_EDGE ( 'NONE', *, *, #8671, .T. ) ;
#9758 = ORIENTED_EDGE ( 'NONE', *, *, #9412, .T. ) ;
#9759 = CARTESIAN_POINT ( 'NONE',  ( -22.99999999999959854, -19.33065833018789803, -21.50000000000000000 ) ) ;
#9760 = ORIENTED_EDGE ( 'NONE', *, *, #3358, .T. ) ;
#9761 = APPROVAL_DATE_TIME ( #11780, #211 ) ;
#9762 = ORIENTED_EDGE ( 'NONE', *, *, #3740, .F. ) ;
#9763 = VERTEX_POINT ( 'NONE', #8575 ) ;
#9764 = CARTESIAN_POINT ( 'NONE',  ( 2.499999999999987566, -17.30000000000000782, 5.000000000000000000 ) ) ;
#9765 = DATE_AND_TIME ( #17242, #6531 ) ;
#9766 = CARTESIAN_POINT ( 'NONE',  ( -20.00000000000000000, -20.00000000000000000, 0.000000000000000000 ) ) ;
#9767 = EDGE_CURVE ( 'NONE', #21997, #17836, #5693, .T. ) ;
#9768 = CARTESIAN_POINT ( 'NONE',  ( -21.99941224366415682, -0.1563100308134309779, -5.000000000000000000 ) ) ;
#9769 = AXIS2_PLACEMENT_3D ( 'NONE', #13880, #5314, #19465 ) ;
#9770 = VECTOR ( 'NONE', #19287, 1000.000000000000000 ) ;
#9771 = DIRECTION ( 'NONE',  ( 0.2306359803922031215, 0.9730401042858034533, -4.741332172907939802E-18 ) ) ;
#9772 = SECURITY_CLASSIFICATION_LEVEL ( 'unclassified' ) ;
#9773 = VERTEX_POINT ( 'NONE', #10367 ) ;
#9774 = AXIS2_PLACEMENT_3D ( 'NONE', #19984, #14752, #21764 ) ;
#9775 = CARTESIAN_POINT ( 'NONE',  ( -16.50082286259682363, 23.02797946379152094, -5.000000000000000000 ) ) ;
#9776 = CARTESIAN_POINT ( 'NONE',  ( 39.76749112244890227, 5.702509466636369595, -15.50000000000000000 ) ) ;
#9777 = ORIENTED_EDGE ( 'NONE', *, *, #1729, .T. ) ;
#9778 = AXIS2_PLACEMENT_3D ( 'NONE', #13042, #5435, #10922 ) ;
#9779 = CIRCLE ( 'NONE', #1415, 2.500000000000000444 ) ;
#9780 = DIRECTION ( 'NONE',  ( 0.2306359803922085339, 0.9730401042858022320, 0.000000000000000000 ) ) ;
#9781 = CARTESIAN_POINT ( 'NONE',  ( -14.70588235717680092, 25.77561860482770228, -7.999999999996769695 ) ) ;
#9782 = ORIENTED_EDGE ( 'NONE', *, *, #19974, .T. ) ;
#9783 = LINE ( 'NONE', #17005, #19447 ) ;
#9784 = PERSON_AND_ORGANIZATION ( #11966, #8758 ) ;
#9785 = VERTEX_POINT ( 'NONE', #956 ) ;
#9786 = VERTEX_POINT ( 'NONE', #17362 ) ;
#9787 = CARTESIAN_POINT ( 'NONE',  ( -27.00000000000000000, -31.09999999999999787, 6.250000000000000000 ) ) ;
#9788 = DIRECTION ( 'NONE',  ( -6.123237831918399306E-17, 2.152213273084510109E-30, 1.000000000000000000 ) ) ;
#9789 = ORIENTED_EDGE ( 'NONE', *, *, #18986, .T. ) ;
#9790 = PERSON_AND_ORGANIZATION ( #11966, #8758 ) ;
#9791 = LINE ( 'NONE', #20699, #3166 ) ;
#9792 = EDGE_CURVE ( 'NONE', #18951, #11427, #22002, .T. ) ;
#9793 = LINE ( 'NONE', #20813, #12066 ) ;
#9794 = DATE_AND_TIME ( #18582, #20993 ) ;
#9795 = CARTESIAN_POINT ( 'NONE',  ( 55.46237324781409939, -8.294657213477510282, -13.00000000000000000 ) ) ;
#9796 = CIRCLE ( 'NONE', #8262, 2.499999999999998668 ) ;
#9797 = CIRCLE ( 'NONE', #23041, 2.066999999999998394 ) ;
#9798 = DIRECTION ( 'NONE',  ( 3.959184095919419975E-16, -4.969292347292200534E-15, -1.000000000000000000 ) ) ;
#9799 = EDGE_CURVE ( 'NONE', #18216, #16983, #6790, .T. ) ;
#9800 = ADVANCED_FACE ( 'NONE', ( #10244 ), #8214, .T. ) ;
#9801 = CARTESIAN_POINT ( 'NONE',  ( 5.000000000000000000, -23.36217782649100272, 2.500000000000000000 ) ) ;
#9802 = PERSON_AND_ORGANIZATION ( #11966, #8758 ) ;
#9803 = CARTESIAN_POINT ( 'NONE',  ( -70.63306599754589854, 6.130251853413639651, 3.000000000000100364 ) ) ;
#9804 = CONICAL_SURFACE ( 'NONE', #18515, 5.386751345948120218, 1.047197551196598297 ) ;
#9805 = DIRECTION ( 'NONE',  ( -0.9080662505692100872, 0.4188265566761218417, -1.040834085574018826E-15 ) ) ;
#9806 = CARTESIAN_POINT ( 'NONE',  ( -27.50000000434389946, 26.95208919188010199, -5.499999999993869793 ) ) ;
#9807 = DIRECTION ( 'NONE',  ( -0.04564792618500997101, -0.9989575901083128651, 2.775557561562890562E-15 ) ) ;
#9808 = CIRCLE ( 'NONE', #15859, 7.999999999999998224 ) ;
#9809 = CARTESIAN_POINT ( 'NONE',  ( -20.00000000397360012, 22.95208919256889857, -2.500000000000039968 ) ) ;
#9810 = ORIENTED_EDGE ( 'NONE', *, *, #19215, .T. ) ;
#9811 = VERTEX_POINT ( 'NONE', #15445 ) ;
#9812 = CARTESIAN_POINT ( 'NONE',  ( 59.43368109719860826, 4.124228161845699958, 3.772686752615189359E-14 ) ) ;
#9813 = VECTOR ( 'NONE', #19978, 999.9999999999998863 ) ;
#9814 = DIRECTION ( 'NONE',  ( 0.2306359803922080898, 0.9730401042858024541, -2.572202231434325988E-16 ) ) ;
#9815 = EDGE_LOOP ( 'NONE', ( #19202, #15668 ) ) ;
#9816 = ADVANCED_FACE ( 'NONE', ( #15697 ), #22680, .T. ) ;
#9817 = ORIENTED_EDGE ( 'NONE', *, *, #11707, .T. ) ;
#9818 = DIRECTION ( 'NONE',  ( -0.9730401042858022320, 0.2306359803922080343, 5.959266323858941219E-17 ) ) ;
#9819 = SECURITY_CLASSIFICATION_LEVEL ( 'unclassified' ) ;
#9820 = FACE_OUTER_BOUND ( 'NONE', #463, .T. ) ;
#9821 = CC_DESIGN_PERSON_AND_ORGANIZATION_ASSIGNMENT ( #19113, #10089, ( #5893 ) ) ;
#9822 = CC_DESIGN_PERSON_AND_ORGANIZATION_ASSIGNMENT ( #561, #18766, ( #8325 ) ) ;
#9823 = CALENDAR_DATE ( 2026, 31, 10 ) ;
#9824 =( LENGTH_UNIT ( ) NAMED_UNIT ( * ) SI_UNIT ( .MILLI., .METRE. ) );
#9825 = DIRECTION ( 'NONE',  ( 0.2306359803921919083, 0.9730401042858062288, 8.673617379884073337E-14 ) ) ;
#9826 = EDGE_CURVE ( 'NONE', #22663, #21240, #13308, .T. ) ;
#9827 = EDGE_CURVE ( 'NONE', #20287, #14097, #20206, .T. ) ;
#9828 = EDGE_CURVE ( 'NONE', #17589, #16214, #7242, .T. ) ;
#9829 = AXIS2_PLACEMENT_3D ( 'NONE', #19146, #10126, #21032 ) ;
#9830 = CARTESIAN_POINT ( 'NONE',  ( 63.71761976613755962, -9.737513338266090557, 1.037827268014797219E-14 ) ) ;
#9831 = ORIENTED_EDGE ( 'NONE', *, *, #22234, .F. ) ;
#9832 = DIRECTION ( 'NONE',  ( 1.138590270679730064E-14, 2.220446049251240387E-15, 1.000000000000000000 ) ) ;
#9833 = FACE_OUTER_BOUND ( 'NONE', #14914, .T. ) ;
#9834 = VERTEX_POINT ( 'NONE', #2753 ) ;
#9835 = DIRECTION ( 'NONE',  ( 2.561207961876604989E-14, 0.000000000000000000, -1.000000000000000000 ) ) ;
#9836 = DIRECTION ( 'NONE',  ( -3.210834492181049985E-17, 2.441916418604790135E-15, 1.000000000000000000 ) ) ;
#9837 = VERTEX_POINT ( 'NONE', #4997 ) ;
#9838 = UNCERTAINTY_MEASURE_WITH_UNIT (LENGTH_MEASURE( 1.000000000000000082E-05 ), #2432, 'distance_accuracy_value', 'NONE');
#9839 = PERSON_AND_ORGANIZATION_ROLE ( 'classification_officer' ) ;
#9840 = FACE_OUTER_BOUND ( 'NONE', #12805, .T. ) ;
#9841 = VERTEX_POINT ( 'NONE', #836 ) ;
#9842 = DATE_AND_TIME ( #9479, #18645 ) ;
#9843 = CARTESIAN_POINT ( 'NONE',  ( -25.00842861987481314, -15.87143667223275401, -21.50000000000000000 ) ) ;
#9844 = ADVANCED_FACE ( 'NONE', ( #6553 ), #20502, .T. ) ;
#9845 = VERTEX_POINT ( 'NONE', #8109 ) ;
#9846 = ORIENTED_EDGE ( 'NONE', *, *, #3124, .T. ) ;
#9847 = CALENDAR_DATE ( 2026, 31, 10 ) ;
#9848 = MANIFOLD_SOLID_BREP ( 'Imported1', #22396 ) ;
#9849 = PERSON_AND_ORGANIZATION ( #19549, #7636 ) ;
#9850 = CARTESIAN_POINT ( 'NONE',  ( 38.79430841974229338, 19.80722199214049084, -13.00000000000049916 ) ) ;
#9851 = CC_DESIGN_APPROVAL ( #4295, ( #6812 ) ) ;
#9852 = CIRCLE ( 'NONE', #1480, 2.499999999999999112 ) ;
#9853 = EDGE_CURVE ( 'NONE', #23033, #1637, #6424, .T. ) ;
#9854 = ADVANCED_FACE ( 'NONE', ( #6311 ), #21142, .T. ) ;
#9855 = DIRECTION ( 'NONE',  ( 1.000000000000000000, -5.964507377817269296E-17, 0.000000000000000000 ) ) ;
#9856 = EDGE_LOOP ( 'NONE', ( #5881, #3420, #19141, #19026 ) ) ;
#9857 = PERSON_AND_ORGANIZATION_ROLE ( 'creator' ) ;
#9858 = ORIENTED_EDGE ( 'NONE', *, *, #6600, .T. ) ;
#9859 = DIRECTION ( 'NONE',  ( -1.000000000000000000, -6.662111140531837817E-09, 1.144917494144693313E-14 ) ) ;
#9860 = FACE_OUTER_BOUND ( 'NONE', #2954, .T. ) ;
#9861 = EDGE_LOOP ( 'NONE', ( #280, #10472, #11089, #9891 ) ) ;
#9862 = FACE_BOUND ( 'NONE', #6245, .T. ) ;
#9863 = CYLINDRICAL_SURFACE ( 'NONE', #22516, 2.500000000000001332 ) ;
#9864 = DIRECTION ( 'NONE',  ( -9.594916218540590128E-33, 2.583840697242805182E-16, -1.000000000000000000 ) ) ;
#9865 = ORIENTED_EDGE ( 'NONE', *, *, #7623, .F. ) ;
#9866 = ORIENTED_EDGE ( 'NONE', *, *, #5781, .F. ) ;
#9868 = CIRCLE ( 'NONE', #5306, 2.500000000000000000 ) ;
#9867 = CARTESIAN_POINT ( 'NONE',  ( 43.81897180516431689, 0.03336243584794939404, -21.50000000000000000 ) ) ;
#9869 = EDGE_LOOP ( 'NONE', ( #20231, #716, #23259, #10791 ) ) ;
#9870 = COORDINATED_UNIVERSAL_TIME_OFFSET ( 0, 0, .AHEAD. ) ;
#9871 = EDGE_CURVE ( 'NONE', #12983, #8958, #4885, .T. ) ;
#9872 = EDGE_LOOP ( 'NONE', ( #8288, #9846, #12578, #19432 ) ) ;
#9873 = VERTEX_POINT ( 'NONE', #10023 ) ;
#9874 = CARTESIAN_POINT ( 'NONE',  ( -26.68810977484059777, -6.639828994528159889, -8.572666733291279949E-14 ) ) ;
#9875 = APPROVAL_STATUS ( 'not_yet_approved' ) ;
#9876 = CYLINDRICAL_SURFACE ( 'NONE', #10511, 2.499999999999998668 ) ;
#9877 = EDGE_CURVE ( 'NONE', #404, #17065, #1536, .T. ) ;
#9878 = FACE_OUTER_BOUND ( 'NONE', #14460, .T. ) ;
#9879 = EDGE_CURVE ( 'NONE', #18433, #7459, #16325, .T. ) ;
#9880 = ADVANCED_FACE ( 'NONE', ( #1659, #11272 ), #23145, .T. ) ;
#9881 = LOCAL_TIME ( 14, 11, 27.00000000000000000, #5926 ) ;
#9882 =( NAMED_UNIT ( * ) SI_UNIT ( $, .STERADIAN. ) SOLID_ANGLE_UNIT ( ) );
#9883 = CC_DESIGN_APPROVAL ( #15157, ( #10620 ) ) ;
#9884 = CIRCLE ( 'NONE', #21236, 2.499999999999998668 ) ;
#9885 = DIRECTION ( 'NONE',  ( -0.1630842657209329583, -0.6880432561069529385, 0.7071067811865517916 ) ) ;
#9886 = CALENDAR_DATE ( 2026, 31, 10 ) ;
#9887 = ORIENTED_EDGE ( 'NONE', *, *, #13905, .F. ) ;
#9888 = DIRECTION ( 'NONE',  ( -0.2306359803922009288, -0.9730401042858040084, 0.000000000000000000 ) ) ;
#9889 = CARTESIAN_POINT ( 'NONE',  ( 30.16078946048219933, 0.07586793050052280385, 13.00000000000019895 ) ) ;
#9890 = AXIS2_PLACEMENT_3D ( 'NONE', #13702, #2784, #21171 ) ;
#9891 = ORIENTED_EDGE ( 'NONE', *, *, #13044, .T. ) ;
#9892 = CARTESIAN_POINT ( 'NONE',  ( 34.67470932959370344, 24.53963568513860238, -11.00000000000049916 ) ) ;
#9893 = DIRECTION ( 'NONE',  ( 1.138590270679734009E-14, 2.220446049251240387E-15, 1.000000000000000000 ) ) ;
#9894 = AXIS2_PLACEMENT_3D ( 'NONE', #11212, #14853, #16402 ) ;
#9895 = EDGE_LOOP ( 'NONE', ( #994, #14212, #9725, #3828 ) ) ;
#9896 = LINE ( 'NONE', #6318, #20941 ) ;
#9897 = APPLICATION_CONTEXT ( 'configuration controlled 3d designs of mechanical parts and assemblies' ) ;
#9898 = COORDINATED_UNIVERSAL_TIME_OFFSET ( 0, 0, .AHEAD. ) ;
#9899 = PRODUCT_DEFINITION_SHAPE ( 'NONE', 'NONE',  #23487 ) ;
#9900 = CC_DESIGN_APPROVAL ( #211, ( #8957 ) ) ;
#9901 = VERTEX_POINT ( 'NONE', #10835 ) ;
#9902 = ORIENTED_EDGE ( 'NONE', *, *, #21893, .T. ) ;
#9903 = CARTESIAN_POINT ( 'NONE',  ( 11.50000000000000000, -23.36217782649120167, 2.500000000000000000 ) ) ;
#9904 = CARTESIAN_POINT ( 'NONE',  ( 36.50043006307940630, 22.92019839501199741, -13.00000000000030020 ) ) ;
#9905 = APPROVAL_PERSON_ORGANIZATION ( #5748, #5101, #18588 ) ;
#9906 = ORIENTED_EDGE ( 'NONE', *, *, #5950, .T. ) ;
#9907 = CALENDAR_DATE ( 2026, 31, 10 ) ;
#9908 = APPROVAL ( #10747, 'UNSPECIFIED' ) ;
#9909 = DIRECTION ( 'NONE',  ( -0.9730401042858022320, 0.2306359803922080343, 5.959266323858941219E-17 ) ) ;
#9910 = LINE ( 'NONE', #17136, #6471 ) ;
#9911 = APPROVAL_DATE_TIME ( #8237, #14153 ) ;
#9912 = DIRECTION ( 'NONE',  ( -1.000000000000000000, 0.000000000000000000, 0.000000000000000000 ) ) ;
#9913 = CLOSED_SHELL ( 'NONE', ( #2204, #6514, #14587, #19654, #19450, #8485, #14576, #13174, #19916, #20531, #13401, #9197, #9673, #18421, #2011, #9854, #9880, #23141, #13616, #6955 ) ) ;
#9914 = DIRECTION ( 'NONE',  ( -0.9730401042858035643, 0.2306359803922028717, 5.958148513035547083E-17 ) ) ;
#9915 = COORDINATED_UNIVERSAL_TIME_OFFSET ( 0, 0, .AHEAD. ) ;
#9916 = LOCAL_TIME ( 14, 11, 27.00000000000000000, #11908 ) ;
#9917 = SECURITY_CLASSIFICATION ( '', '', #22592 ) ;
#9918 = LINE ( 'NONE', #5876, #8514 ) ;
#9919 = LINE ( 'NONE', #11359, #4474 ) ;
#9921 = DIRECTION ( 'NONE',  ( 2.982858504489129897E-17, -2.441916418604790135E-15, -1.000000000000000000 ) ) ;
#9920 = VECTOR ( 'NONE', #2341, 1000.000000000000000 ) ;
#9922 = ADVANCED_FACE ( 'NONE', ( #10715, #21599 ), #16148, .F. ) ;
#9923 = LINE ( 'NONE', #6345, #13321 ) ;
#9924 = LOCAL_TIME ( 14, 11, 27.00000000000000000, #20744 ) ;
#9925 = DIRECTION ( 'NONE',  ( 0.9730401042858036753, -0.2306359803922031493, -5.959266323858673745E-17 ) ) ;
#9926 = SECURITY_CLASSIFICATION ( '', '', #14224 ) ;
#9927 = DIRECTION ( 'NONE',  ( 0.2306359803922031215, 0.9730401042858035643, 4.620383928407073520E-16 ) ) ;
#9928 = AXIS2_PLACEMENT_3D ( 'NONE', #6985, #20980, #10195 ) ;
#9929 = VERTEX_POINT ( 'NONE', #14251 ) ;
#9930 = PERSON ( 'NAUO-PER31', 'UNSPECIFIED', 'UNSPECIFIED', ('UNSPECIFIED'), ('UNSPECIFIED'), ('UNSPECIFIED') ) ;
#9931 = EDGE_LOOP ( 'NONE', ( #20294, #17443, #9123, #1537 ) ) ;
#9932 = DIRECTION ( 'NONE',  ( 0.000000000000000000, 0.000000000000000000, -1.000000000000000000 ) ) ;
#9933 = FACE_OUTER_BOUND ( 'NONE', #20277, .T. ) ;
#9934 = ORIENTED_EDGE ( 'NONE', *, *, #10562, .T. ) ;
#9935 = ADVANCED_FACE ( 'NONE', ( #14805 ), #12375, .F. ) ;
#9936 = ADVANCED_FACE ( 'NONE', ( #17715 ), #9469, .F. ) ;
#9937 = FACE_OUTER_BOUND ( 'NONE', #10028, .T. ) ;
#9938 = ORIENTED_EDGE ( 'NONE', *, *, #9557, .T. ) ;
#9939 = SECURITY_CLASSIFICATION ( '', '', #7099 ) ;
#9940 = PLANE ( 'NONE',  #2263 ) ;
#9941 = SECURITY_CLASSIFICATION ( '', '', #15803 ) ;
#9942 = PERSON_AND_ORGANIZATION_ROLE ( 'creator' ) ;
#9943 = AXIS2_PLACEMENT_3D ( 'NONE', #13075, #11307, #14958 ) ;
#9944 = CARTESIAN_POINT ( 'NONE',  ( 114.8178196092480050, -22.36345201740209987, 20.00000000000000000 ) ) ;
#9945 = VECTOR ( 'NONE', #16398, 1000.000000000000114 ) ;
#9946 = APPROVAL_DATE_TIME ( #13254, #15592 ) ;
#9947 = DIRECTION ( 'NONE',  ( 0.000000000000000000, 0.000000000000000000, 1.000000000000000000 ) ) ;
#9948 = CC_DESIGN_SECURITY_CLASSIFICATION ( #12599, ( #23499 ) ) ;
#9949 = DIRECTION ( 'NONE',  ( 0.000000000000000000, -1.000000000000000000, 2.081668171172168119E-15 ) ) ;
#9950 = DIRECTION ( 'NONE',  ( 0.000000000000000000, 1.000000000000000000, -9.248890187689720549E-11 ) ) ;
#9951 = DIRECTION ( 'NONE',  ( -0.9730401042858022320, 0.2306359803922080343, 5.959266323858941219E-17 ) ) ;
#9952 = ORIENTED_EDGE ( 'NONE', *, *, #13580, .T. ) ;
#9953 = CARTESIAN_POINT ( 'NONE',  ( -30.79248430819469817, 6.338858557518999959, 5.500000000000089706 ) ) ;
#9954 = EDGE_CURVE ( 'NONE', #1222, #2277, #15960, .T. ) ;
#9955 = APPROVAL_PERSON_ORGANIZATION ( #15796, #15623, #19241 ) ;
#9956 = ORIENTED_EDGE ( 'NONE', *, *, #13236, .F. ) ;
#9957 = CARTESIAN_POINT ( 'NONE',  ( 117.0319250210129951, -13.02226701625849969, -18.89999999999999858 ) ) ;
#9958 = AXIS2_PLACEMENT_3D ( 'NONE', #6823, #10166, #8496 ) ;
#9959 = LINE ( 'NONE', #10079, #9920 ) ;
#9960 = APPROVAL ( #12053, 'UNKNOWN' ) ;
#9961 = PERSON_AND_ORGANIZATION ( #7642, #827 ) ;
#9962 = AXIS2_PLACEMENT_3D ( 'NONE', #5914, #7579, #16706 ) ;
#9963 = CC_DESIGN_DATE_AND_TIME_ASSIGNMENT ( #17487, #13927, ( #11475 ) ) ;
#9964 = CIRCLE ( 'NONE', #3500, 7.999999999999997335 ) ;
#9965 = CARTESIAN_POINT ( 'NONE',  ( -20.00000000397080058, 22.95208919256900160, 8.500000000004460432 ) ) ;
#9966 = LOCAL_TIME ( 14, 11, 27.00000000000000000, #14696 ) ;
#9967 = ORIENTED_EDGE ( 'NONE', *, *, #9271, .F. ) ;
#9968 = ADVANCED_FACE ( 'NONE', ( #1534 ), #12604, .F. ) ;
#9969 = EDGE_CURVE ( 'NONE', #1465, #3741, #16037, .T. ) ;
#9970 = COORDINATED_UNIVERSAL_TIME_OFFSET ( 0, 0, .AHEAD. ) ;
#9971 = DIRECTION ( 'NONE',  ( -0.5021071549687922131, 0.8648054144888001060, 0.000000000000000000 ) ) ;
#9972 = ORIENTED_EDGE ( 'NONE', *, *, #17227, .F. ) ;
#9973 = ORIENTED_EDGE ( 'NONE', *, *, #17047, .T. ) ;
#9974 = VECTOR ( 'NONE', #16985, 1000.000000000000227 ) ;
#9975 = DIRECTION ( 'NONE',  ( 0.000000000000000000, 0.000000000000000000, -1.000000000000000000 ) ) ;
#9976 = APPROVAL_DATE_TIME ( #20646, #1243 ) ;
#9977 = EDGE_CURVE ( 'NONE', #7018, #8336, #398, .T. ) ;
#9978 = SECURITY_CLASSIFICATION ( '', '', #18282 ) ;
#9979 = SECURITY_CLASSIFICATION_LEVEL ( 'unclassified' ) ;
#9980 = DIRECTION ( 'NONE',  ( 0.2306359803922076457, 0.9730401042858023430, 0.000000000000000000 ) ) ;
#9981 = AXIS2_PLACEMENT_3D ( 'NONE', #6914, #5473, #18301 ) ;
#9982 = CIRCLE ( 'NONE', #4285, 15.25000000000000000 ) ;
#9983 = VECTOR ( 'NONE', #7790, 1000.000000000000000 ) ;
#9984 = DIRECTION ( 'NONE',  ( 0.000000000000000000, 0.000000000000000000, -1.000000000000000000 ) ) ;
#9985 = EDGE_LOOP ( 'NONE', ( #18452, #12188, #3542, #7494 ) ) ;
#9986 = AXIS2_PLACEMENT_3D ( 'NONE', #21300, #5041, #22714 ) ;
#9987 = PERSON_AND_ORGANIZATION ( #11966, #8758 ) ;
#9988 = EDGE_CURVE ( 'NONE', #10039, #22602, #22039, .T. ) ;
#9989 = EDGE_LOOP ( 'NONE', ( #21085, #13878 ) ) ;
#9990 = VECTOR ( 'NONE', #565, 999.9999999999998863 ) ;
#9991 = CARTESIAN_POINT ( 'NONE',  ( -20.00000000000000000, -20.00000000000000000, 5.500000000004559020 ) ) ;
#9992 = LINE ( 'NONE', #2157, #8974 ) ;
#9993 = VERTEX_POINT ( 'NONE', #13152 ) ;
#9994 = APPROVAL ( #11434, 'UNSPECIFIED' ) ;
#9995 = LOCAL_TIME ( 14, 11, 27.00000000000000000, #12683 ) ;
#9996 = LINE ( 'NONE', #4110, #10565 ) ;
#9997 = CC_DESIGN_PERSON_AND_ORGANIZATION_ASSIGNMENT ( #8092, #4399, ( #1883 ) ) ;
#9998 = DIRECTION ( 'NONE',  ( 2.270069654138865127E-15, 1.000000000000000000, -4.543838814073030634E-30 ) ) ;
#9999 = CYLINDRICAL_SURFACE ( 'NONE', #14142, 2.500000000000000000 ) ;
#10000 = EDGE_LOOP ( 'NONE', ( #17522, #13992 ) ) ;
#10001 = ORIENTED_EDGE ( 'NONE', *, *, #7777, .F. ) ;
#10002 = DIRECTION ( 'NONE',  ( 0.2306359803922053142, 0.9730401042858028982, 0.000000000000000000 ) ) ;
#10003 = AXIS2_PLACEMENT_3D ( 'NONE', #18656, #5688, #20659 ) ;
#10004 = ORIENTED_EDGE ( 'NONE', *, *, #19682, .T. ) ;
#10005 = EDGE_CURVE ( 'NONE', #1110, #14624, #5, .T. ) ;
#10006 = EDGE_CURVE ( 'NONE', #300, #14758, #23273, .T. ) ;
#10007 = CALENDAR_DATE ( 2026, 31, 10 ) ;
#10008 = VERTEX_POINT ( 'NONE', #5229 ) ;
#10009 = AXIS2_PLACEMENT_3D ( 'NONE', #15584, #4783, #12736 ) ;
#10010 = ORIENTED_EDGE ( 'NONE', *, *, #6305, .F. ) ;
#10011 = DIRECTION ( 'NONE',  ( 0.000000000000000000, 0.000000000000000000, 1.000000000000000000 ) ) ;
#10012 = APPROVAL_DATE_TIME ( #5702, #12713 ) ;
#10013 = CYLINDRICAL_SURFACE ( 'NONE', #3274, 2.067000000000000171 ) ;
#10014 = VECTOR ( 'NONE', #3841, 999.9999999999998863 ) ;
#10015 = DIRECTION ( 'NONE',  ( -0.005235963827108352890, 0.9999862922474493931, 5.936218956694023463E-19 ) ) ;
#10016 = AXIS2_PLACEMENT_3D ( 'NONE', #1069, #4095, #9699 ) ;
#10017 = VECTOR ( 'NONE', #17839, 1000.000000000000114 ) ;
#10018 = DIRECTION ( 'NONE',  ( 0.1630842657209349289, 0.6880432561069608211, 0.7071067811865437980 ) ) ;
#10019 = PERSON_AND_ORGANIZATION_ROLE ( 'creator' ) ;
#10020 = ADVANCED_FACE ( 'NONE', ( #16264 ), #5341, .T. ) ;
#10021 = CIRCLE ( 'NONE', #21754, 3.750000000000000000 ) ;
#10022 = ORIENTED_EDGE ( 'NONE', *, *, #11641, .F. ) ;
#10023 = CARTESIAN_POINT ( 'NONE',  ( -25.44839750738890061, 25.46504853262630164, -5.000000000000070166 ) ) ;
#10024 = DIRECTION ( 'NONE',  ( -0.9730401042858035643, 0.2306359803922028717, 5.667427308550587516E-17 ) ) ;
#10025 = ORIENTED_EDGE ( 'NONE', *, *, #5841, .T. ) ;
#10026 = DIRECTION ( 'NONE',  ( -2.269747459788994803E-13, -2.220446049250325308E-15, -1.000000000000000000 ) ) ;
#10027 = DIRECTION ( 'NONE',  ( 1.085472681297010170E-15, 4.321163532573060300E-15, 1.000000000000000000 ) ) ;
#10028 = EDGE_LOOP ( 'NONE', ( #3205, #9391 ) ) ;
#10029 = AXIS2_PLACEMENT_3D ( 'NONE', #6925, #10144, #21049 ) ;
#10030 = CARTESIAN_POINT ( 'NONE',  ( 36.07092311366588433, 11.78608357701227760, 19.56699999999998951 ) ) ;
#10031 = EDGE_CURVE ( 'NONE', #18157, #6518, #6096, .T. ) ;
#10032 = APPROVAL_STATUS ( 'not_yet_approved' ) ;
#10033 = CIRCLE ( 'NONE', #16060, 1.749999999999997780 ) ;
#10035 = EDGE_CURVE ( 'NONE', #6050, #1008, #769, .T. ) ;
#10034 = VERTEX_POINT ( 'NONE', #13045 ) ;
#10036 = EDGE_LOOP ( 'NONE', ( #21953, #9147, #1989, #2752 ) ) ;
#10037 = CARTESIAN_POINT ( 'NONE',  ( 117.0319250210129951, -13.02226701625859917, 15.90000000000000036 ) ) ;
#10038 = CARTESIAN_POINT ( 'NONE',  ( -20.00000000397270128, 22.95208919257159863, 5.000000000004460432 ) ) ;
#10039 = VERTEX_POINT ( 'NONE', #15915 ) ;
#10040 = AXIS2_PLACEMENT_3D ( 'NONE', #7598, #2243, #16386 ) ;
#10041 = PERSON_AND_ORGANIZATION_ROLE ( 'creator' ) ;
#10042 = FACE_BOUND ( 'NONE', #13365, .T. ) ;
#10043 = DIRECTION ( 'NONE',  ( 1.159535895544890222E-14, 2.167612681253619929E-15, 1.000000000000000000 ) ) ;
#10044 = APPROVAL_ROLE ( '' ) ;
#10045 = CYLINDRICAL_SURFACE ( 'NONE', #22274, 3.499999999999998224 ) ;
#10046 = DIRECTION ( 'NONE',  ( 0.5249589903860194529, -0.8511275218278935295, 5.444325428271645316E-17 ) ) ;
#10047 = COORDINATED_UNIVERSAL_TIME_OFFSET ( 0, 0, .AHEAD. ) ;
#10048 = AXIS2_PLACEMENT_3D ( 'NONE', #1949, #10782, #22010 ) ;
#10049 = CARTESIAN_POINT ( 'NONE',  ( 35.24899100468473989, 7.732362805529279903, 8.759424124906640685 ) ) ;
#10050 = VECTOR ( 'NONE', #3306, 1000.000000000000000 ) ;
#10051 = CARTESIAN_POINT ( 'NONE',  ( 122.4288069621910040, 9.746871424029301068, 13.00000000000000000 ) ) ;
#10052 = CC_DESIGN_DATE_AND_TIME_ASSIGNMENT ( #15695, #4648, ( #12504 ) ) ;
#10053 = CARTESIAN_POINT ( 'NONE',  ( 29.87858131747766421, 2.137125494442374318, -13.00000000000039968 ) ) ;
#10054 = CARTESIAN_POINT ( 'NONE',  ( -32.42710143188249816, 10.33427914179039853, 2.500000000000000000 ) ) ;
#10055 = FACE_OUTER_BOUND ( 'NONE', #18599, .T. ) ;
#10056 = CYLINDRICAL_SURFACE ( 'NONE', #20184, 7.000000000000004441 ) ;
#10057 = EDGE_LOOP ( 'NONE', ( #2496, #2473, #15546, #23286, #15696, #21228 ) ) ;
#10058 = ORIENTED_EDGE ( 'NONE', *, *, #7511, .F. ) ;
#10059 = DIRECTION ( 'NONE',  ( 0.000000000000000000, 0.000000000000000000, 1.000000000000000000 ) ) ;
#10060 = CARTESIAN_POINT ( 'NONE',  ( 30.57814311865390167, -3.583136841840119935, -15.00000000000039968 ) ) ;
#10061 = ORIENTED_EDGE ( 'NONE', *, *, #10830, .T. ) ;
#10062 = DIRECTION ( 'NONE',  ( 0.1630842657209343738, 0.6880432561069577124, -0.7071067811865469066 ) ) ;
#10063 = VERTEX_POINT ( 'NONE', #6261 ) ;
#10064 = CARTESIAN_POINT ( 'NONE',  ( 114.1489752661110089, -25.18526831983109915, 3.000000000000000000 ) ) ;
#10065 = PERSON_AND_ORGANIZATION ( #11966, #8758 ) ;
#10066 = CARTESIAN_POINT ( 'NONE',  ( -20.00000000397080058, 22.95208919256900160, 8.500000000004460432 ) ) ;
#10067 = EDGE_CURVE ( 'NONE', #16708, #18951, #8280, .T. ) ;
#10068 = PERSON_AND_ORGANIZATION_ROLE ( 'classification_officer' ) ;
#10069 = LINE ( 'NONE', #13607, #16794 ) ;
#10070 = DIRECTION ( 'NONE',  ( -0.005235963827110212514, 0.9999862922474493931, 6.182393958678891872E-17 ) ) ;
#10071 = DIRECTION ( 'NONE',  ( 1.000000000000000000, 0.000000000000000000, 0.000000000000000000 ) ) ;
#10072 = CYLINDRICAL_SURFACE ( 'NONE', #7737, 2.499999999999998668 ) ;
#10073 = EDGE_LOOP ( 'NONE', ( #13153, #1816 ) ) ;
#10074 = CARTESIAN_POINT ( 'NONE',  ( -20.00000000397270128, 22.95208919256889857, -5.499999999995559996 ) ) ;
#10075 = AXIS2_PLACEMENT_3D ( 'NONE', #570, #15174, #22537 ) ;
#10076 = LINE ( 'NONE', #11857, #19006 ) ;
#10077 = ORIENTED_EDGE ( 'NONE', *, *, #4585, .F. ) ;
#10078 = DIRECTION ( 'NONE',  ( -0.8660135325225011282, -0.004534477687572232088, -0.4999999999999998890 ) ) ;
#10079 = CARTESIAN_POINT ( 'NONE',  ( 5.000000000000000000, -23.36217782649100272, 2.500000000000000000 ) ) ;
#10080 = COORDINATED_UNIVERSAL_TIME_OFFSET ( 0, 0, .AHEAD. ) ;
#10081 = CYLINDRICAL_SURFACE ( 'NONE', #8442, 6.000000000001507239 ) ;
#10082 = ORIENTED_EDGE ( 'NONE', *, *, #22989, .T. ) ;
#10083 = VERTEX_POINT ( 'NONE', #11386 ) ;
#10084 = DATE_TIME_ROLE ( 'creation_date' ) ;
#10085 = DIRECTION ( 'NONE',  ( 1.138590270679730064E-14, 2.220446049251235259E-15, 1.000000000000000000 ) ) ;
#10086 = ORIENTED_EDGE ( 'NONE', *, *, #23404, .T. ) ;
#10087 = FACE_BOUND ( 'NONE', #13876, .T. ) ;
#10088 =( REPRESENTATION_RELATIONSHIP ('NONE','NONE', #19303, #4731 ) REPRESENTATION_RELATIONSHIP_WITH_TRANSFORMATION ( #14680 )SHAPE_REPRESENTATION_RELATIONSHIP( ) );
#10089 = PERSON_AND_ORGANIZATION_ROLE ( 'creator' ) ;
#10090 = ADVANCED_FACE ( 'NONE', ( #2817 ), #15280, .T. ) ;
#10091 = DATE_AND_TIME ( #21005, #9166 ) ;
#10092 = SHAPE_REPRESENTATION ( '1602p_c_33', ( #12739 ), #20868 ) ;
#10093 = PLANE ( 'NONE',  #22946 ) ;
#10094 = CC_DESIGN_PERSON_AND_ORGANIZATION_ASSIGNMENT ( #11971, #1119, ( #1200 ) ) ;
#10095 = FACE_OUTER_BOUND ( 'NONE', #5450, .T. ) ;
#10096 = VERTEX_POINT ( 'NONE', #4363 ) ;
#10097 = ADVANCED_FACE ( 'NONE', ( #22522 ), #3445, .F. ) ;
#10098 = EDGE_CURVE ( 'NONE', #22078, #8396, #13694, .T. ) ;
#10099 = SECURITY_CLASSIFICATION_LEVEL ( 'unclassified' ) ;
#10100 = PRODUCT ( '1602p_c_12', '1602p_c_12', '', ( #6535 ) ) ;
#10101 = EDGE_LOOP ( 'NONE', ( #22992, #3460 ) ) ;
#10102 = CARTESIAN_POINT ( 'NONE',  ( 114.8178196092480050, -22.36345201740219935, -13.00000000000000000 ) ) ;
#10103 = FACE_OUTER_BOUND ( 'NONE', #21128, .T. ) ;
#10104 = EDGE_LOOP ( 'NONE', ( #12245, #8056, #8173, #28 ) ) ;
#10105 = DIRECTION ( 'NONE',  ( -0.9999862922474492821, -0.005235963827121953122, 1.187304881134294758E-16 ) ) ;
#10106 = DIRECTION ( 'NONE',  ( -1.000000000000000000, -6.662111140531837817E-09, 1.144917494144693313E-14 ) ) ;
#10107 = CARTESIAN_POINT ( 'NONE',  ( -1.540112692620030144, -27.34999999999999787, 2.500000000000000000 ) ) ;
#10108 = ORIENTED_EDGE ( 'NONE', *, *, #1482, .F. ) ;
#10109 = ORIENTED_EDGE ( 'NONE', *, *, #14311, .F. ) ;
#10110 = DIRECTION ( 'NONE',  ( 3.210834492194344756E-17, -2.441916418604790135E-15, -1.000000000000000000 ) ) ;
#10111 = ORIENTED_EDGE ( 'NONE', *, *, #9214, .T. ) ;
#10112 = PERSON_AND_ORGANIZATION ( #11966, #8758 ) ;
#10113 = CIRCLE ( 'NONE', #12743, 2.501000000000000334 ) ;
#10114 = ORIENTED_EDGE ( 'NONE', *, *, #5400, .F. ) ;
#10115 = VERTEX_POINT ( 'NONE', #18859 ) ;
#10116 = FACE_OUTER_BOUND ( 'NONE', #19725, .T. ) ;
#10117 = COORDINATED_UNIVERSAL_TIME_OFFSET ( 0, 0, .AHEAD. ) ;
#10118 = EDGE_CURVE ( 'NONE', #11037, #11043, #13503, .T. ) ;
#10119 = CARTESIAN_POINT ( 'NONE',  ( 35.59419854219520118, 9.774809681453239918, -37.44562646538079775 ) ) ;
#10120 = APPROVAL ( #15769, 'UNSPECIFIED' ) ;
#10121 = AXIS2_PLACEMENT_3D ( 'NONE', #1742, #14347, #23471 ) ;
#10122 = CC_DESIGN_DATE_AND_TIME_ASSIGNMENT ( #3052, #17554, ( #16771 ) ) ;
#10123 = CIRCLE ( 'NONE', #21483, 5.000000000000000000 ) ;
#10124 = ADVANCED_FACE ( 'NONE', ( #18967 ), #17189, .F. ) ;
#10125 = EDGE_CURVE ( 'NONE', #3393, #8685, #8066, .T. ) ;
#10126 = DIRECTION ( 'NONE',  ( -0.9730401042858036753, 0.2306359803922031493, 5.432877459303543355E-17 ) ) ;
#10127 = COORDINATED_UNIVERSAL_TIME_OFFSET ( 0, 0, .AHEAD. ) ;
#10128 = APPROVAL ( #21155, 'UNSPECIFIED' ) ;
#10129 = EDGE_LOOP ( 'NONE', ( #1225, #1720, #12742, #2949, #5656 ) ) ;
#10130 = CARTESIAN_POINT ( 'NONE',  ( 35.59419854219520118, 9.774809681453278998, 21.49999999999999289 ) ) ;
#10131 = DIRECTION ( 'NONE',  ( 0.005235963827117092427, -0.9999862922474493931, -2.636227439667000721E-16 ) ) ;
#10132 = ORIENTED_EDGE ( 'NONE', *, *, #14272, .F. ) ;
#10133 = CARTESIAN_POINT ( 'NONE',  ( -5.303405830673253440, 11.24695771925867760, -1.731061307250961080E-15 ) ) ;
#10134 = FACE_OUTER_BOUND ( 'NONE', #11493, .T. ) ;
#10135 = CARTESIAN_POINT ( 'NONE',  ( -26.17677262429019791, 24.41614710630589968, 2.500000000000000000 ) ) ;
#10136 = ORIENTED_EDGE ( 'NONE', *, *, #3748, .T. ) ;
#10137 = CARTESIAN_POINT ( 'NONE',  ( 117.1933702072879981, -12.34113894325849969, 19.59999999999999787 ) ) ;
#10138 = APPROVAL_DATE_TIME ( #7993, #5175 ) ;
#10139 = AXIS2_PLACEMENT_3D ( 'NONE', #17527, #8268, #11844 ) ;
#10140 = EDGE_LOOP ( 'NONE', ( #196, #1766, #8557, #11290 ) ) ;
#10141 = ORIENTED_EDGE ( 'NONE', *, *, #13641, .F. ) ;
#10142 = DIRECTION ( 'NONE',  ( -1.000000000000000000, 2.275047181608926658E-16, 0.000000000000000000 ) ) ;
#10143 = VECTOR ( 'NONE', #20286, 999.9999999999998863 ) ;
#10144 = DIRECTION ( 'NONE',  ( -0.9730401042858035643, 0.2306359803922028717, 5.958148513035547083E-17 ) ) ;
#10145 = VECTOR ( 'NONE', #5144, 1000.000000000000000 ) ;
#10146 = VERTEX_POINT ( 'NONE', #2579 ) ;
#10147 = APPROVAL_DATE_TIME ( #6223, #6450 ) ;
#10148 = DIRECTION ( 'NONE',  ( 5.101515458763229339E-16, 0.000000000000000000, 1.000000000000000000 ) ) ;
#10149 = ADVANCED_FACE ( 'NONE', ( #9833 ), #11518, .F. ) ;
#10150 = EDGE_CURVE ( 'NONE', #12003, #22438, #2464, .T. ) ;
#10151 = DIRECTION ( 'NONE',  ( -0.2306359803922080620, -0.9730401042858023430, -1.901827233595000632E-14 ) ) ;
#10152 = ITEM_DEFINED_TRANSFORMATION ( 'NONE', 'NONE', #16683,  #12739 ) ;
#10153 = DIRECTION ( 'NONE',  ( 3.099353312215989243E-62, -1.534091707905539548E-92, -1.000000000000000000 ) ) ;
#10154 = AXIS2_PLACEMENT_3D ( 'NONE', #16292, #16076, #14283 ) ;
#10155 = EDGE_CURVE ( 'NONE', #19234, #11874, #20131, .T. ) ;
#10156 = DIRECTION ( 'NONE',  ( -2.982858504489129897E-17, 2.441916418604790135E-15, 1.000000000000000000 ) ) ;
#10157 = PERSON_AND_ORGANIZATION_ROLE ( 'classification_officer' ) ;
#10158 = CIRCLE ( 'NONE', #17351, 2.500000000028978597 ) ;
#10159 = EDGE_CURVE ( 'NONE', #17438, #13418, #12548, .T. ) ;
#10160 = VECTOR ( 'NONE', #22803, 1000.000000000000000 ) ;
#10161 = CARTESIAN_POINT ( 'NONE',  ( 37.66475682276774251, 9.836590499361282269, 8.984920035094594581 ) ) ;
#10162 = CARTESIAN_POINT ( 'NONE',  ( 118.6002496876800052, -6.405594307115080710, -18.89999999999999858 ) ) ;
#10163 = PLANE ( 'NONE',  #20730 ) ;
#10164 = CARTESIAN_POINT ( 'NONE',  ( 3.174494135099829695, 19.69896361837129817, 4.500000000000000000 ) ) ;
#10165 = CIRCLE ( 'NONE', #1400, 7.999999999999997335 ) ;
#10166 = DIRECTION ( 'NONE',  ( 2.269747459788999852E-13, 2.220446049250475192E-15, 1.000000000000000000 ) ) ;
#10167 = DIRECTION ( 'NONE',  ( -1.000000000000000000, 0.000000000000000000, 0.000000000000000000 ) ) ;
#10168 = ORIENTED_EDGE ( 'NONE', *, *, #4906, .T. ) ;
#10169 = ORIENTED_EDGE ( 'NONE', *, *, #5050, .T. ) ;
#10170 = CARTESIAN_POINT ( 'NONE',  ( -27.00000000000000000, -20.00000000000000000, -2.500000000000000000 ) ) ;
#10171 = DIRECTION ( 'NONE',  ( -3.210834492181045054E-17, 2.441916418604790135E-15, 1.000000000000000000 ) ) ;
#10172 = AXIS2_PLACEMENT_3D ( 'NONE', #17955, #5471, #21492 ) ;
#10173 = EDGE_LOOP ( 'NONE', ( #6270, #17918, #15057, #2881 ) ) ;
#10174 = DIRECTION ( 'NONE',  ( 0.6660003063074656504, -0.7459514675891198987, 0.000000000000000000 ) ) ;
#10175 = CIRCLE ( 'NONE', #13195, 2.500000000000000000 ) ;
#10176 = ORIENTED_EDGE ( 'NONE', *, *, #1218, .F. ) ;
#10177 = CIRCLE ( 'NONE', #23411, 1.250000000000000222 ) ;
#10178 = CARTESIAN_POINT ( 'NONE',  ( -30.72441677844230057, -6.660963241697680282, -3.000000000000079936 ) ) ;
#10179 = AXIS2_PLACEMENT_3D ( 'NONE', #4437, #13933, #1092 ) ;
#10180 = MECHANICAL_CONTEXT ( 'NONE', #16698, 'mechanical' ) ;
#10181 = CARTESIAN_POINT ( 'NONE',  ( -14.00000000202540029, 1.899127378930379972, 8.000000000004439116 ) ) ;
#10182 = EDGE_CURVE ( 'NONE', #22935, #3926, #5708, .T. ) ;
#10183 = APPROVAL_ROLE ( '' ) ;
#10184 = EDGE_CURVE ( 'NONE', #8396, #1694, #10076, .T. ) ;
#10185 = SHAPE_REPRESENTATION_RELATIONSHIP ( 'NONE' , 'NONE' ,  #17646, #3978 ) ;
#10186 = VECTOR ( 'NONE', #10207, 1000.000000000000000 ) ;
#10187 = DIRECTION ( 'NONE',  ( -1.000000000000000000, -9.259491321837100239E-11, 2.269596547736281384E-13 ) ) ;
#10188 = EDGE_CURVE ( 'NONE', #9834, #14253, #1007, .T. ) ;
#10189 = DIRECTION ( 'NONE',  ( 1.000000000000000000, -1.053068847079585977E-24, -1.138589415280572122E-14 ) ) ;
#10190 = DIRECTION ( 'NONE',  ( 0.000000000000000000, 0.000000000000000000, 1.000000000000000000 ) ) ;
#10191 = CIRCLE ( 'NONE', #8665, 5.000000000000000888 ) ;
#10192 = LINE ( 'NONE', #14203, #11190 ) ;
#10193 = ORIENTED_EDGE ( 'NONE', *, *, #5223, .F. ) ;
#10194 = LINE ( 'NONE', #12331, #266 ) ;
#10195 = DIRECTION ( 'NONE',  ( -0.9730401042858022320, 0.2306359803922080343, 1.051187380996432105E-30 ) ) ;
#10196 = AXIS2_PLACEMENT_3D ( 'NONE', #19396, #2893, #22704 ) ;
#10197 = VERTEX_POINT ( 'NONE', #22744 ) ;
#10198 = CARTESIAN_POINT ( 'NONE',  ( 33.69273454209145768, 8.920130599203270449, -8.912036319352662161 ) ) ;
#10199 = DIRECTION ( 'NONE',  ( 0.9730401042858035643, -0.2306359803922028717, -5.432877459303547053E-17 ) ) ;
#10200 = CALENDAR_DATE ( 2026, 31, 10 ) ;
#10201 = LINE ( 'NONE', #23337, #14519 ) ;
#10202 = ORIENTED_EDGE ( 'NONE', *, *, #23294, .T. ) ;
#10203 = EDGE_LOOP ( 'NONE', ( #13041, #19124, #10849, #22540 ) ) ;
#10204 = DATE_TIME_ROLE ( 'classification_date' ) ;
#10205 = LINE ( 'NONE', #8171, #22063 ) ;
#10206 = ORIENTED_EDGE ( 'NONE', *, *, #5951, .T. ) ;
#10207 = DIRECTION ( 'NONE',  ( -2.269747459789000104E-13, -2.220446049250330436E-15, -1.000000000000000000 ) ) ;
#10208 = APPROVAL_DATE_TIME ( #13632, #16471 ) ;
#10209 = CIRCLE ( 'NONE', #11354, 2.500000000000000888 ) ;
#10210 = CARTESIAN_POINT ( 'NONE',  ( 58.73439644601037912, 17.65016624305025061, 15.00923999999996461 ) ) ;
#10211 = LINE ( 'NONE', #1151, #15289 ) ;
#10212 = VERTEX_POINT ( 'NONE', #13737 ) ;
#10213 =( REPRESENTATION_RELATIONSHIP ('NONE','NONE', #18121, #20540 ) REPRESENTATION_RELATIONSHIP_WITH_TRANSFORMATION ( #12596 )SHAPE_REPRESENTATION_RELATIONSHIP( ) );
#10214 = VERTEX_POINT ( 'NONE', #22275 ) ;
#10215 = CARTESIAN_POINT ( 'NONE',  ( -59.85533902005759899, -24.86725927682059734, -5.000000000000000000 ) ) ;
#10216 = DIRECTION ( 'NONE',  ( 0.5249589903860232276, -0.8511275218278909760, 1.971684378104701054E-16 ) ) ;
#10218 = VERTEX_POINT ( 'NONE', #2338 ) ;
#10217 = EDGE_CURVE ( 'NONE', #54, #4836, #14823, .T. ) ;
#10219 = EDGE_CURVE ( 'NONE', #9718, #11739, #4590, .T. ) ;
#10220 = CARTESIAN_POINT ( 'NONE',  ( -20.00000000000000000, -20.00000000000000000, 5.500000000004559020 ) ) ;
#10221 = LINE ( 'NONE', #582, #3569 ) ;
#10222 = DIRECTION ( 'NONE',  ( 0.000000000000000000, 0.000000000000000000, -1.000000000000000000 ) ) ;
#10223 = VERTEX_POINT ( 'NONE', #6850 ) ;
#10224 = ORIENTED_EDGE ( 'NONE', *, *, #11010, .T. ) ;
#10225 = CARTESIAN_POINT ( 'NONE',  ( 41.17437060284130013, 11.63805410277969976, 20.00000000000000000 ) ) ;
#10226 = ORIENTED_EDGE ( 'NONE', *, *, #12770, .T. ) ;
#10227 = COORDINATED_UNIVERSAL_TIME_OFFSET ( 0, 0, .AHEAD. ) ;
#10228 = EDGE_LOOP ( 'NONE', ( #19844, #13112, #3927, #9130, #21606 ) ) ;
#10229 = ORIENTED_EDGE ( 'NONE', *, *, #9439, .F. ) ;
#10230 = CYLINDRICAL_SURFACE ( 'NONE', #13753, 2.500000000028980374 ) ;
#10231 =( BOUNDED_CURVE ( )  B_SPLINE_CURVE ( 2, ( #11396, #18633, #2829 ),
 .UNSPECIFIED., .F., .F. ) 
 B_SPLINE_CURVE_WITH_KNOTS ( ( 3, 3 ),
 ( 0.000000000000000000, 0.2336872276155859962 ),
 .UNSPECIFIED. ) 
 CURVE ( )  GEOMETRIC_REPRESENTATION_ITEM ( )  RATIONAL_B_SPLINE_CURVE ( ( 1.000000000000000000, 1.154700538379259900, 1.000000000000000000 ) ) 
 REPRESENTATION_ITEM ( '' )  );
#10232 = APPLICATION_PROTOCOL_DEFINITION ( 'international standard', 'config_control_design', 1994, #5972 ) ;
#10233 = CIRCLE ( 'NONE', #3424, 5.000000000000002665 ) ;
#10234 = ADVANCED_FACE ( 'NONE', ( #14208 ), #1256, .T. ) ;
#10235 = EDGE_CURVE ( 'NONE', #6625, #12797, #15567, .T. ) ;
#10236 = CARTESIAN_POINT ( 'NONE',  ( 48.79336017845105999, 1.507728449240719915, 3.776618445270551233E-14 ) ) ;
#10237 =( NAMED_UNIT ( * ) PLANE_ANGLE_UNIT ( ) SI_UNIT ( $, .RADIAN. ) );
#10238 = FACE_BOUND ( 'NONE', #13887, .T. ) ;
#10239 = CARTESIAN_POINT ( 'NONE',  ( 14.29185906324030064, 14.82402186575814085, -3.345896859062374887E-15 ) ) ;
#10240 = APPLICATION_PROTOCOL_DEFINITION ( 'international standard', 'config_control_design', 1994, #13979 ) ;
#10241 = PRODUCT ( '1602p_c_46', '1602p_c_46', '', ( #13826 ) ) ;
#10242 = ORIENTED_EDGE ( 'NONE', *, *, #4811, .T. ) ;
#10243 = LOCAL_TIME ( 14, 11, 27.00000000000000000, #19050 ) ;
#10244 = FACE_OUTER_BOUND ( 'NONE', #7226, .T. ) ;
#10245 = AXIS2_PLACEMENT_3D ( 'NONE', #21426, #3367, #3016 ) ;
#10246 = CARTESIAN_POINT ( 'NONE',  ( 29.89447396975359794, -1.047702001783030079, -15.00000000000039968 ) ) ;
#10247 = EDGE_LOOP ( 'NONE', ( #13191, #22782, #5762, #2614, #19890, #18054, #8930, #6408 ) ) ;
#10248 = EDGE_CURVE ( 'NONE', #16249, #17065, #1128, .T. ) ;
#10249 = DIRECTION ( 'NONE',  ( -2.982858504577319616E-17, 2.441916418604790135E-15, 1.000000000000000000 ) ) ;
#10250 = CARTESIAN_POINT ( 'NONE',  ( 35.09206298776550170, 20.88063091279819972, 13.00000000000000000 ) ) ;
#10251 = FACE_BOUND ( 'NONE', #13484, .T. ) ;
#10252 = ORIENTED_EDGE ( 'NONE', *, *, #21315, .F. ) ;
#10253 = DIRECTION ( 'NONE',  ( 1.000000000000000000, 0.000000000000000000, 1.480297366166879989E-16 ) ) ;
#10254 = APPROVAL ( #1877, 'UNKNOWN' ) ;
#10255 = SECURITY_CLASSIFICATION_LEVEL ( 'unclassified' ) ;
#10256 = ORIENTED_EDGE ( 'NONE', *, *, #15630, .F. ) ;
#10257 = CC_DESIGN_PERSON_AND_ORGANIZATION_ASSIGNMENT ( #9402, #23399, ( #11856 ) ) ;
#10258 = ORIENTED_EDGE ( 'NONE', *, *, #18976, .T. ) ;
#10259 = CARTESIAN_POINT ( 'NONE',  ( 27.87922736721089834, -4.130116823142910398, 13.00000000000019895 ) ) ;
#10260 = CARTESIAN_POINT ( 'NONE',  ( 37.10730959030829723, 23.96304573415820016, 15.00000000000000000 ) ) ;
#10261 = FACE_BOUND ( 'NONE', #15959, .T. ) ;
#10262 = APPROVAL_ROLE ( '' ) ;
#10263 = EDGE_CURVE ( 'NONE', #13655, #15538, #11015, .T. ) ;
#10264 = CARTESIAN_POINT ( 'NONE',  ( -19.99999999999809930, -20.00000000000000000, 8.500000000004551026 ) ) ;
#10265 = ADVANCED_FACE ( 'NONE', ( #12430 ), #3384, .F. ) ;
#10266 = DIRECTION ( 'NONE',  ( 4.063875459488295522E-16, -1.011971878839177951E-16, -1.000000000000000000 ) ) ;
#10267 = AXIS2_PLACEMENT_3D ( 'NONE', #8859, #9072, #10884 ) ;
#10268 =( GEOMETRIC_REPRESENTATION_CONTEXT ( 3 ) GLOBAL_UNCERTAINTY_ASSIGNED_CONTEXT ( ( #18206 ) ) GLOBAL_UNIT_ASSIGNED_CONTEXT ( ( #16749, #16514, #481 ) ) REPRESENTATION_CONTEXT ( 'NONE', 'WORKASPACE' ) );
#10269 = AXIS2_PLACEMENT_3D ( 'NONE', #17961, #21608, #19609 ) ;
#10270 = PLANE ( 'NONE',  #6360 ) ;
#10271 = VECTOR ( 'NONE', #14524, 1000.000000000000000 ) ;
#10272 = CARTESIAN_POINT ( 'NONE',  ( -25.00842861987479893, -15.87143667223269894, -25.00000000000000000 ) ) ;
#10273 = APPROVAL_ROLE ( '' ) ;
#10274 = CARTESIAN_POINT ( 'NONE',  ( 37.67179450110460692, -4.077824265976569329, 13.00000000000000000 ) ) ;
#10275 = CARTESIAN_POINT ( 'NONE',  ( 120.8143550994449953, 2.935590694028629599, 20.00000000000000000 ) ) ;
#10276 = CARTESIAN_POINT ( 'NONE',  ( -62.86014019962070165, -2.329165347875060021, -5.524798807282839984E-15 ) ) ;
#10277 = EDGE_CURVE ( 'NONE', #10416, #965, #3775, .T. ) ;
#10278 = LOCAL_TIME ( 14, 11, 27.00000000000000000, #15229 ) ;
#10279 = DIRECTION ( 'NONE',  ( 0.000000000000000000, 0.000000000000000000, -1.000000000000000000 ) ) ;
#10280 = LINE ( 'NONE', #12305, #16000 ) ;
#10281 = APPROVAL_PERSON_ORGANIZATION ( #979, #12792, #22831 ) ;
#10282 = ORIENTED_EDGE ( 'NONE', *, *, #8338, .F. ) ;
#10283 = FACE_OUTER_BOUND ( 'NONE', #20564, .T. ) ;
#10284 = ORIENTED_EDGE ( 'NONE', *, *, #22177, .T. ) ;
#10285 = ORIENTED_EDGE ( 'NONE', *, *, #18353, .T. ) ;
#10286 = LINE ( 'NONE', #1106, #2757 ) ;
#10287 = DIRECTION ( 'NONE',  ( 0.2306359803922031215, 0.9730401042858034533, -4.741332172907939802E-18 ) ) ;
#10288 = ORIENTED_EDGE ( 'NONE', *, *, #19639, .T. ) ;
#10289 = AXIS2_PLACEMENT_3D ( 'NONE', #3574, #10597, #8803 ) ;
#10290 = EDGE_CURVE ( 'NONE', #1981, #14140, #1600, .T. ) ;
#10291 = PLANE ( 'NONE',  #19076 ) ;
#10292 = EDGE_CURVE ( 'NONE', #13768, #22084, #12211, .T. ) ;
#10293 = VERTEX_POINT ( 'NONE', #16102 ) ;
#10294 = CARTESIAN_POINT ( 'NONE',  ( 122.7747609327790030, 11.20643158045800014, 9.133960000000000079 ) ) ;
#10295 = APPROVAL_STATUS ( 'not_yet_approved' ) ;
#10296 = DIRECTION ( 'NONE',  ( 0.2306359803922080343, 0.9730401042858022320, -1.015202274805050187E-13 ) ) ;
#10297 = CC_DESIGN_SECURITY_CLASSIFICATION ( #1527, ( #14812 ) ) ;
#10298 = ITEM_DEFINED_TRANSFORMATION ( 'NONE', 'NONE', #9110,  #12739 ) ;
#10299 = DIRECTION ( 'NONE',  ( 1.000000000000000000, 0.000000000000000000, 0.000000000000000000 ) ) ;
#10300 = CC_DESIGN_SECURITY_CLASSIFICATION ( #1155, ( #8384 ) ) ;
#10301 = CARTESIAN_POINT ( 'NONE',  ( -20.00000000000000000, -22.50000000000000000, -5.499999999995464073 ) ) ;
#10302 = AXIS2_PLACEMENT_3D ( 'NONE', #1744, #18272, #7352 ) ;
#10303 = CARTESIAN_POINT ( 'NONE',  ( -16.50000000144740042, -4.350228928666989958, 5.500000000004489742 ) ) ;
#10304 = LOCAL_TIME ( 14, 11, 27.00000000000000000, #22984 ) ;
#10305 = CARTESIAN_POINT ( 'NONE',  ( -20.00000000000149925, -20.00000000000000000, -6.749999999995469402 ) ) ;
#10306 = ORIENTED_EDGE ( 'NONE', *, *, #10691, .T. ) ;
#10308 = VECTOR ( 'NONE', #525, 1000.000000000000000 ) ;
#10307 = CARTESIAN_POINT ( 'NONE',  ( 86.89068504225697609, -31.09999999999999787, -21.49999999999999645 ) ) ;
#10309 = EDGE_CURVE ( 'NONE', #21101, #6563, #19551, .T. ) ;
#10310 = CARTESIAN_POINT ( 'NONE',  ( 31.11077410011089839, -1.335996977273280262, -11.00000000000039968 ) ) ;
#10311 = ORIENTED_EDGE ( 'NONE', *, *, #83, .T. ) ;
#10312 = CARTESIAN_POINT ( 'NONE',  ( 35.80338916065181820, 11.83562432877527471, -8.762640180330977913 ) ) ;
#10313 = DIRECTION ( 'NONE',  ( -0.9730401042858035643, 0.2306359803922028717, 5.432877459303547053E-17 ) ) ;
#10314 = ORIENTED_EDGE ( 'NONE', *, *, #18745, .T. ) ;
#10315 = CC_DESIGN_SECURITY_CLASSIFICATION ( #14070, ( #23156 ) ) ;
#10316 = APPROVAL_STATUS ( 'not_yet_approved' ) ;
#10317 = LINE ( 'NONE', #3392, #4261 ) ;
#10318 = CC_DESIGN_APPROVAL ( #17427, ( #2323 ) ) ;
#10319 = ORIENTED_EDGE ( 'NONE', *, *, #15038, .F. ) ;
#10320 = EDGE_LOOP ( 'NONE', ( #19852, #4193, #5620, #18520, #1320, #5935 ) ) ;
#10321 = AXIS2_PLACEMENT_3D ( 'NONE', #3651, #19577, #16125 ) ;
#10322 = ADVANCED_FACE ( 'NONE', ( #19201 ), #17771, .T. ) ;
#10323 = CALENDAR_DATE ( 2026, 31, 10 ) ;
#10324 = DIRECTION ( 'NONE',  ( -6.281952996264290168E-17, -4.969341027148640384E-15, -1.000000000000000000 ) ) ;
#10325 = ORIENTED_EDGE ( 'NONE', *, *, #3237, .T. ) ;
#10326 = EDGE_CURVE ( 'NONE', #503, #3857, #1879, .T. ) ;
#10327 = DIRECTION ( 'NONE',  ( -0.9730401042858022320, 0.2306359803922080343, 5.959266323858941219E-17 ) ) ;
#10328 = ORGANIZATION ( 'NAUO-ORG18', 'UNSPECIFIED', 'UNSPECIFIED' ) ;
#10329 = PERSON_AND_ORGANIZATION ( #11966, #8758 ) ;
#10330 = SECURITY_CLASSIFICATION_LEVEL ( 'unclassified' ) ;
#10331 = LINE ( 'NONE', #21349, #17662 ) ;
#10332 = CC_DESIGN_APPROVAL ( #16473, ( #18531 ) ) ;
#10333 = CARTESIAN_POINT ( 'NONE',  ( 37.10730959030829723, 23.96304573415810069, -15.00000000000049916 ) ) ;
#10334 = EDGE_LOOP ( 'NONE', ( #4352, #17605, #16132, #1871 ) ) ;
#10335 = EDGE_LOOP ( 'NONE', ( #2462, #8655, #1960, #1125 ) ) ;
#10336 = AXIS2_PLACEMENT_3D ( 'NONE', #18738, #6007, #20144 ) ;
#10337 = DIRECTION ( 'NONE',  ( -0.2306359803922028440, -0.9730401042858034533, -4.307366329831518561E-32 ) ) ;
#10338 = CARTESIAN_POINT ( 'NONE',  ( 58.25686728443101003, 17.76335315678745630, -15.50000000000049916 ) ) ;
#10339 = ORIENTED_EDGE ( 'NONE', *, *, #4811, .F. ) ;
#10340 = CC_DESIGN_PERSON_AND_ORGANIZATION_ASSIGNMENT ( #628, #20354, ( #19526 ) ) ;
#10341 = CARTESIAN_POINT ( 'NONE',  ( -0.03403376487617969931, 6.499910899608420500, -2.500000000000090150 ) ) ;
#10342 = LINE ( 'NONE', #4975, #10050 ) ;
#10343 = CARTESIAN_POINT ( 'NONE',  ( 38.02679880290970971, 9.198219730472773747, -26.30000000000049809 ) ) ;
#10344 = ORIENTED_EDGE ( 'NONE', *, *, #15022, .T. ) ;
#10345 = VERTEX_POINT ( 'NONE', #8877 ) ;
#10346 = CARTESIAN_POINT ( 'NONE',  ( -62.93786153767959490, 12.51438117767279934, -2.729132938682636844 ) ) ;
#10347 = ORIENTED_EDGE ( 'NONE', *, *, #21176, .F. ) ;
#10348 = CALENDAR_DATE ( 2026, 31, 10 ) ;
#10349 = PRODUCT_DEFINITION_FORMATION_WITH_SPECIFIED_SOURCE ( 'ANY', '', #4728, .NOT_KNOWN. ) ;
#10350 = ORIENTED_EDGE ( 'NONE', *, *, #18076, .F. ) ;
#10351 = EDGE_LOOP ( 'NONE', ( #604, #18842, #10580, #6257 ) ) ;
#10352 = LINE ( 'NONE', #4986, #6546 ) ;
#10353 = PERSON_AND_ORGANIZATION ( #11966, #8758 ) ;
#10354 = AXIS2_PLACEMENT_3D ( 'NONE', #19265, #14028, #19497 ) ;
#10355 = CONICAL_SURFACE ( 'NONE', #464, 2.624999999999998668, 0.4636476090008101458 ) ;
#10356 = AXIS2_PLACEMENT_3D ( 'NONE', #2937, #2590, #9971 ) ;
#10357 = CYLINDRICAL_SURFACE ( 'NONE', #14651, 3.999999999999998668 ) ;
#10358 = AXIS2_PLACEMENT_3D ( 'NONE', #3738, #5286, #12547 ) ;
#10359 = ORIENTED_EDGE ( 'NONE', *, *, #15947, .T. ) ;
#10360 = APPLICATION_CONTEXT ( 'configuration controlled 3d designs of mechanical parts and assemblies' ) ;
#10361 = AXIS2_PLACEMENT_3D ( 'NONE', #23153, #6432, #962 ) ;
#10362 = EDGE_CURVE ( 'NONE', #3647, #10223, #19431, .T. ) ;
#10363 = DIRECTION ( 'NONE',  ( -1.000000000000000000, 0.000000000000000000, 0.000000000000000000 ) ) ;
#10364 = COORDINATED_UNIVERSAL_TIME_OFFSET ( 0, 0, .AHEAD. ) ;
#10365 = LOCAL_TIME ( 14, 11, 27.00000000000000000, #21345 ) ;
#10366 = ORIENTED_EDGE ( 'NONE', *, *, #11880, .T. ) ;
#10367 = CARTESIAN_POINT ( 'NONE',  ( 43.45766680872420551, 21.27115113520920175, 20.00000000000000000 ) ) ;
#10368 = AXIS2_PLACEMENT_3D ( 'NONE', #11901, #8192, #17092 ) ;
#10369 = CARTESIAN_POINT ( 'NONE',  ( 122.4288069621910040, 9.746871424029221131, -10.02499999999999858 ) ) ;
#10370 = VERTEX_POINT ( 'NONE', #7089 ) ;
#10371 = VECTOR ( 'NONE', #16808, 1000.000000000000227 ) ;
#10372 = DIRECTION ( 'NONE',  ( -0.2306359803922084506, -0.9730401042858020100, 5.112869192352694760E-15 ) ) ;
#10373 = AXIS2_PLACEMENT_3D ( 'NONE', #7556, #15021, #11839 ) ;
#10374 = FACE_OUTER_BOUND ( 'NONE', #10104, .T. ) ;
#10375 = SHAPE_REPRESENTATION ( '1602p_c_23', ( #12739 ), #4017 ) ;
#10376 = CARTESIAN_POINT ( 'NONE',  ( 30.57814311865390167, -3.583136841840119935, -11.00000000000039968 ) ) ;
#10377 = VERTEX_POINT ( 'NONE', #8629 ) ;
#10378 = DIRECTION ( 'NONE',  ( -0.9730401042858024541, 0.2306359803922080898, 5.959266323858942451E-17 ) ) ;
#10379 = DATE_AND_TIME ( #22812, #12560 ) ;
#10380 = ORIENTED_EDGE ( 'NONE', *, *, #16218, .T. ) ;
#10381 = VERTEX_POINT ( 'NONE', #15634 ) ;
#10382 = LINE ( 'NONE', #1198, #17585 ) ;
#10383 = CARTESIAN_POINT ( 'NONE',  ( -30.72441677844210162, -6.660963241697129611, -2.999000000000090260 ) ) ;
#10384 = VECTOR ( 'NONE', #22618, 1000.000000000000114 ) ;
#10385 = CARTESIAN_POINT ( 'NONE',  ( -20.11411981943522775, 20.45469521730081652, 5.000000000004466649 ) ) ;
#10386 = APPROVAL_ROLE ( '' ) ;
#10387 = AXIS2_PLACEMENT_3D ( 'NONE', #7949, #2717, #13179 ) ;
#10388 = CARTESIAN_POINT ( 'NONE',  ( 36.30836311812279860, 20.59233593730800038, 13.00000000000000000 ) ) ;
#10389 = LOCAL_TIME ( 14, 11, 27.00000000000000000, #12320 ) ;
#10390 = DIRECTION ( 'NONE',  ( 0.7107421451278728153, -0.7034526303448085383, -8.700833610568998825E-17 ) ) ;
#10391 = VECTOR ( 'NONE', #6291, 999.9999999999998863 ) ;
#10392 = DIRECTION ( 'NONE',  ( -2.269747459788994803E-13, -2.220446049250320181E-15, -1.000000000000000000 ) ) ;
#10393 = AXIS2_PLACEMENT_3D ( 'NONE', #19642, #3252, #3365 ) ;
#10394 = ADVANCED_FACE ( 'NONE', ( #2926 ), #15863, .T. ) ;
#10395 = CIRCLE ( 'NONE', #487, 0.4000000000000010214 ) ;
#10396 = DIRECTION ( 'NONE',  ( 0.000000000000000000, 0.000000000000000000, 1.000000000000000000 ) ) ;
#10397 = APPROVAL ( #2344, 'UNKNOWN' ) ;
#10398 = DIRECTION ( 'NONE',  ( 0.005235963827101452160, -0.9999862922474493931, 5.479105319409471602E-16 ) ) ;
#10399 = COORDINATED_UNIVERSAL_TIME_OFFSET ( 0, 0, .AHEAD. ) ;
#10400 = CARTESIAN_POINT ( 'NONE',  ( -25.00000000000000000, -20.00000000000000000, 2.500000000000000000 ) ) ;
#10401 = AXIS2_PLACEMENT_3D ( 'NONE', #13815, #8470, #12389 ) ;
#10402 = CARTESIAN_POINT ( 'NONE',  ( 83.62762864230479920, -14.97056015138839946, -13.00000000000000000 ) ) ;
#10403 = EDGE_CURVE ( 'NONE', #21232, #11204, #17419, .T. ) ;
#10404 = EDGE_CURVE ( 'NONE', #6814, #20686, #17914, .T. ) ;
#10405 = DIRECTION ( 'NONE',  ( -3.638785342205658653E-34, -2.636191302913590118E-16, 1.000000000000000000 ) ) ;
#10406 = CC_DESIGN_SECURITY_CLASSIFICATION ( #6978, ( #23477 ) ) ;
#10407 = FACE_OUTER_BOUND ( 'NONE', #10949, .T. ) ;
#10408 = CYLINDRICAL_SURFACE ( 'NONE', #17906, 6.000000000000109246 ) ;
#10409 = ORIENTED_EDGE ( 'NONE', *, *, #4777, .T. ) ;
#10410 = AXIS2_PLACEMENT_3D ( 'NONE', #1602, #20014, #23450 ) ;
#10411 = PLANE ( 'NONE',  #14890 ) ;
#10412 = AXIS2_PLACEMENT_3D ( 'NONE', #23096, #1485, #15641 ) ;
#10413 = EDGE_LOOP ( 'NONE', ( #20313, #22566, #6556, #3558 ) ) ;
#10414 = LINE ( 'NONE', #2906, #22082 ) ;
#10415 = DIRECTION ( 'NONE',  ( 1.000000000000000000, -3.416070845000479880E-16, 0.000000000000000000 ) ) ;
#10416 = VERTEX_POINT ( 'NONE', #17538 ) ;
#10417 = FACE_OUTER_BOUND ( 'NONE', #1077, .T. ) ;
#10418 = ORIENTED_EDGE ( 'NONE', *, *, #21250, .F. ) ;
#10419 = CYLINDRICAL_SURFACE ( 'NONE', #4937, 2.499999999999998668 ) ;
#10420 = SECURITY_CLASSIFICATION_LEVEL ( 'unclassified' ) ;
#10421 = CARTESIAN_POINT ( 'NONE',  ( -14.00000000000000000, -19.99999999944489915, 6.750000000004490630 ) ) ;
#10422 = EDGE_CURVE ( 'NONE', #2924, #16237, #16213, .T. ) ;
#10423 = VECTOR ( 'NONE', #18717, 1000.000000000000000 ) ;
#10424 = PERSON_AND_ORGANIZATION ( #22673, #8446 ) ;
#10425 = AXIS2_PLACEMENT_3D ( 'NONE', #6926, #5003, #6913 ) ;
#10426 = FACE_OUTER_BOUND ( 'NONE', #13425, .T. ) ;
#10427 = APPROVAL ( #20755, 'UNSPECIFIED' ) ;
#10428 = CARTESIAN_POINT ( 'NONE',  ( -69.83648293172720400, -6.865655411149130138, 7.200000000000000178 ) ) ;
#10429 = DIRECTION ( 'NONE',  ( 0.000000000000000000, 0.000000000000000000, 1.000000000000000000 ) ) ;
#10430 = APPROVAL ( #701, 'UNSPECIFIED' ) ;
#10431 = CARTESIAN_POINT ( 'NONE',  ( 28.41185834866789861, -1.882976958576189963, -16.27970053837969999 ) ) ;
#10432 = ORIENTED_EDGE ( 'NONE', *, *, #8422, .F. ) ;
#10433 = DIRECTION ( 'NONE',  ( 0.000000000000000000, 1.000000000000000000, 0.000000000000000000 ) ) ;
#10434 = EDGE_CURVE ( 'NONE', #18347, #16220, #3511, .T. ) ;
#10435 = EDGE_CURVE ( 'NONE', #8770, #9786, #15479, .T. ) ;
#10436 = DESIGN_CONTEXT ( 'detailed design', #10360, 'design' ) ;
#10437 = DIRECTION ( 'NONE',  ( -0.005235963827117092427, 0.9999862922474493931, 2.636227439667000721E-16 ) ) ;
#10438 = CC_DESIGN_DATE_AND_TIME_ASSIGNMENT ( #2486, #6396, ( #9386 ) ) ;
#10439 = ORIENTED_EDGE ( 'NONE', *, *, #8537, .F. ) ;
#10440 = LINE ( 'NONE', #21329, #2158 ) ;
#10441 = DIRECTION ( 'NONE',  ( 0.000000000000000000, -1.000000000000000000, 0.000000000000000000 ) ) ;
#10442 = ORIENTED_EDGE ( 'NONE', *, *, #12767, .F. ) ;
#10443 = PERSON_AND_ORGANIZATION_ROLE ( 'classification_officer' ) ;
#10444 = CARTESIAN_POINT ( 'NONE',  ( 28.67817383939640052, -0.7594070262926440051, 15.00000000000000000 ) ) ;
#10445 = ORIENTED_EDGE ( 'NONE', *, *, #2742, .T. ) ;
#10446 = EDGE_LOOP ( 'NONE', ( #8574, #20239, #10077, #9482, #10252 ) ) ;
#10447 = DATE_AND_TIME ( #15874, #20159 ) ;
#10448 = DIRECTION ( 'NONE',  ( 0.000000000000000000, 0.000000000000000000, -1.000000000000000000 ) ) ;
#10449 = VERTEX_POINT ( 'NONE', #10787 ) ;
#10450 = CARTESIAN_POINT ( 'NONE',  ( -20.00000000000149925, -20.00000000000000000, -6.499999999995289990 ) ) ;
#10451 = PERSON_AND_ORGANIZATION ( #11966, #8758 ) ;
#10452 = EDGE_CURVE ( 'NONE', #16628, #8168, #20012, .T. ) ;
#10453 = PRODUCT_DEFINITION_SHAPE ( 'NONE', 'NONE',  #4578 ) ;
#10454 = APPROVAL_ROLE ( '' ) ;
#10455 = DIRECTION ( 'NONE',  ( -0.9730401042858020100, 0.2306359803922089780, 0.000000000000000000 ) ) ;
#10456 = ADVANCED_FACE ( 'NONE', ( #21900 ), #11132, .F. ) ;
#10457 = CARTESIAN_POINT ( 'NONE',  ( 33.90884364377009774, 10.17428291754630010, 29.25000000000000000 ) ) ;
#10458 = ORIENTED_EDGE ( 'NONE', *, *, #1857, .F. ) ;
#10459 = EDGE_CURVE ( 'NONE', #357, #15518, #16712, .T. ) ;
#10460 = ADVANCED_FACE ( 'NONE', ( #1719 ), #12670, .T. ) ;
#10461 = EDGE_LOOP ( 'NONE', ( #18573, #12531, #13214, #14193 ) ) ;
#10462 = CARTESIAN_POINT ( 'NONE',  ( 0.03403376487640599746, -6.499910899608420500, 8.873528816395729098E-14 ) ) ;
#10463 = CARTESIAN_POINT ( 'NONE',  ( 113.4570673249340018, -28.10438863268850085, 2.700000000000049916 ) ) ;
#10464 = ORIENTED_EDGE ( 'NONE', *, *, #13020, .T. ) ;
#10465 = CARTESIAN_POINT ( 'NONE',  ( -22.50000000397400157, 22.95208917591821773, -5.499999999995003108 ) ) ;
#10466 = DIRECTION ( 'NONE',  ( 2.269747459789000104E-13, 2.220446049250330436E-15, 1.000000000000000000 ) ) ;
#10467 = ORIENTED_EDGE ( 'NONE', *, *, #22742, .F. ) ;
#10468 = ORIENTED_EDGE ( 'NONE', *, *, #4300, .T. ) ;
#10469 = CARTESIAN_POINT ( 'NONE',  ( -19.99999998648272737, 20.45208919256900160, 8.000000000004465761 ) ) ;
#10470 = EDGE_LOOP ( 'NONE', ( #17233, #11201, #13813, #11397 ) ) ;
#10471 = COORDINATED_UNIVERSAL_TIME_OFFSET ( 0, 0, .AHEAD. ) ;
#10472 = ORIENTED_EDGE ( 'NONE', *, *, #10719, .F. ) ;
#10473 = AXIS2_PLACEMENT_3D ( 'NONE', #3187, #17563, #9980 ) ;
#10474 = ORIENTED_EDGE ( 'NONE', *, *, #10188, .F. ) ;
#10475 = CARTESIAN_POINT ( 'NONE',  ( 28.14554285793940025, -3.006546890859489896, 11.00000000000019895 ) ) ;
#10476 = DATE_AND_TIME ( #6667, #17140 ) ;
#10477 = DIRECTION ( 'NONE',  ( -1.466984912809907930E-16, -2.805478249466195144E-20, -1.000000000000000000 ) ) ;
#10478 = CARTESIAN_POINT ( 'NONE',  ( 40.32424593841290061, 8.051426419082240216, -1.980584223082610025E-14 ) ) ;
#10479 = SECURITY_CLASSIFICATION_LEVEL ( 'unclassified' ) ;
#10480 = AXIS2_PLACEMENT_3D ( 'NONE', #19082, #17413, #22970 ) ;
#10481 = ORIENTED_EDGE ( 'NONE', *, *, #17047, .F. ) ;
#10482 = DIRECTION ( 'NONE',  ( -0.07397971354964408275, -0.9972597464969258363, 2.255140518769849223E-15 ) ) ;
#10483 = DIRECTION ( 'NONE',  ( 0.000000000000000000, 1.156482317317871478E-16, 1.000000000000000000 ) ) ;
#10484 = ORIENTED_EDGE ( 'NONE', *, *, #18394, .T. ) ;
#10485 = AXIS2_PLACEMENT_3D ( 'NONE', #16212, #1951, #19778 ) ;
#10486 = CARTESIAN_POINT ( 'NONE',  ( 34.49867763533223552, 5.152869186095711207, -27.87500000000047606 ) ) ;
#10487 = CARTESIAN_POINT ( 'NONE',  ( -20.00000000397270128, 22.95208919256889857, -4.999999999995559996 ) ) ;
#10488 = CARTESIAN_POINT ( 'NONE',  ( 34.49867763533220710, 5.152869186095990095, 26.88000000000002387 ) ) ;
#10489 = EDGE_LOOP ( 'NONE', ( #16813, #1753, #14748, #17832 ) ) ;
#10490 = DIRECTION ( 'NONE',  ( 0.9730401042858035643, -0.2306359803922028717, -5.959266323858674978E-17 ) ) ;
#10491 = PERSON_AND_ORGANIZATION_ROLE ( 'design_supplier' ) ;
#10492 = ADVANCED_FACE ( 'NONE', ( #3735 ), #18235, .T. ) ;
#10493 = EDGE_LOOP ( 'NONE', ( #1315, #1706, #20406, #19105, #1477 ) ) ;
#10494 = EDGE_LOOP ( 'NONE', ( #8928, #5075, #7956, #7348, #16534 ) ) ;
#10495 = CYLINDRICAL_SURFACE ( 'NONE', #15297, 2.499999999999998668 ) ;
#10496 = LINE ( 'NONE', #15580, #2632 ) ;
#10497 = CARTESIAN_POINT ( 'NONE',  ( 46.46175228317039796, -6.161274394849590053, 13.00000000000000000 ) ) ;
#10498 = APPLICATION_PROTOCOL_DEFINITION ( 'international standard', 'config_control_design', 1994, #11435 ) ;
#10499 = CARTESIAN_POINT ( 'NONE',  ( 0.6139822272806650938, 23.20457113379747938, -7.691623324820558135E-15 ) ) ;
#10500 =( GEOMETRIC_REPRESENTATION_CONTEXT ( 3 ) GLOBAL_UNCERTAINTY_ASSIGNED_CONTEXT ( ( #3249 ) ) GLOBAL_UNIT_ASSIGNED_CONTEXT ( ( #8484, #15476, #22702 ) ) REPRESENTATION_CONTEXT ( 'NONE', 'WORKASPACE' ) );
#10501 = LINE ( 'NONE', #19621, #14807 ) ;
#10502 = CIRCLE ( 'NONE', #22976, 3.499999999999999556 ) ;
#10503 = DIRECTION ( 'NONE',  ( 1.000000000000000000, 0.000000000000000000, 0.000000000000000000 ) ) ;
#10504 = EDGE_LOOP ( 'NONE', ( #12951, #5104, #18616, #19917 ) ) ;
#10505 = DIRECTION ( 'NONE',  ( -6.124317834331790129E-17, 2.578073951808930140E-21, -1.000000000000000000 ) ) ;
#10506 = PERSON_AND_ORGANIZATION_ROLE ( 'classification_officer' ) ;
#10507 =( BOUNDED_CURVE ( )  B_SPLINE_CURVE ( 2, ( #8495, #8250, #21064 ),
 .UNSPECIFIED., .F., .F. ) 
 B_SPLINE_CURVE_WITH_KNOTS ( ( 3, 3 ),
 ( 0.000000000000000000, 0.2336872276155859962 ),
 .UNSPECIFIED. ) 
 CURVE ( )  GEOMETRIC_REPRESENTATION_ITEM ( )  RATIONAL_B_SPLINE_CURVE ( ( 1.000000000000000000, 1.154700538379249908, 1.000000000000000000 ) ) 
 REPRESENTATION_ITEM ( '' )  );
#10508 = CARTESIAN_POINT ( 'NONE',  ( -22.75000000397511002, 22.95208919256900160, -8.499999999994924949 ) ) ;
#10509 = CARTESIAN_POINT ( 'NONE',  ( 52.49909637502329929, -7.592283011512489743, 10.74538000000019800 ) ) ;
#10510 = DIRECTION ( 'NONE',  ( -0.005235963827108352890, 0.9999862922474493931, 5.936218956694023463E-19 ) ) ;
#10511 = AXIS2_PLACEMENT_3D ( 'NONE', #7850, #16988, #706 ) ;
#10512 = DIRECTION ( 'NONE',  ( 0.005235963827110212514, -0.9999862922474493931, -5.936218956700083401E-19 ) ) ;
#10513 = AXIS2_PLACEMENT_3D ( 'NONE', #8843, #11093, #12748 ) ;
#10514 = DIRECTION ( 'NONE',  ( -1.000000000000000000, -9.259433497721235207E-11, 1.142026288351377283E-14 ) ) ;
#10515 = ORIENTED_EDGE ( 'NONE', *, *, #13493, .T. ) ;
#10516 = CARTESIAN_POINT ( 'NONE',  ( 33.27705887009690144, -3.036156860537199798, -13.00000000000039968 ) ) ;
#10517 = EDGE_CURVE ( 'NONE', #12615, #11204, #12150, .T. ) ;
#10518 = EDGE_CURVE ( 'NONE', #8685, #1899, #20334, .T. ) ;
#10519 = ORIENTED_EDGE ( 'NONE', *, *, #3911, .T. ) ;
#10520 = FACE_OUTER_BOUND ( 'NONE', #23043, .T. ) ;
#10521 = CARTESIAN_POINT ( 'NONE',  ( -19.49999999982360066, -0.1021026942259809916, -5.000000000000000000 ) ) ;
#10522 = VERTEX_POINT ( 'NONE', #5281 ) ;
#10523 = CARTESIAN_POINT ( 'NONE',  ( 113.2956221386590130, -28.78551670568859677, -3.100000000000000089 ) ) ;
#10524 = ADVANCED_BREP_SHAPE_REPRESENTATION ( '', ( #1581, #12739 ), #15784 ) ;
#10525 = EDGE_LOOP ( 'NONE', ( #21328, #7898, #12656, #9348 ) ) ;
#10526 = CARTESIAN_POINT ( 'NONE',  ( 35.09747506357100377, 11.43410645592840069, -29.25000000000050093 ) ) ;
#10527 = CIRCLE ( 'NONE', #6738, 0.3999999999999998557 ) ;
#10528 = CALENDAR_DATE ( 2026, 31, 10 ) ;
#10529 = CARTESIAN_POINT ( 'NONE',  ( -26.75617730459320143, 6.359992804688680224, -8.571895024826909188E-14 ) ) ;
#10530 = EDGE_CURVE ( 'NONE', #5291, #21101, #23169, .T. ) ;
#10531 = EDGE_CURVE ( 'NONE', #13456, #16192, #22785, .T. ) ;
#10532 = VECTOR ( 'NONE', #20982, 1000.000000000000000 ) ;
#10533 = AXIS2_PLACEMENT_3D ( 'NONE', #16073, #16290, #3476 ) ;
#10534 = CARTESIAN_POINT ( 'NONE',  ( -19.99999999999819877, -20.00000000000000000, 8.000000000004540368 ) ) ;
#10535 = CARTESIAN_POINT ( 'NONE',  ( -0.2232035960304966093, 20.61124038026003191, -3.168006029165981644E-16 ) ) ;
#10536 = VECTOR ( 'NONE', #3964, 1000.000000000000227 ) ;
#10537 = CARTESIAN_POINT ( 'NONE',  ( -20.00000000000000000, -20.00000000000000000, 6.750000000004559908 ) ) ;
#10538 = ORIENTED_EDGE ( 'NONE', *, *, #21929, .F. ) ;
#10539 = DIRECTION ( 'NONE',  ( -0.9730401042858035643, 0.2306359803922028717, 5.432877459303547053E-17 ) ) ;
#10540 = DIRECTION ( 'NONE',  ( 9.249283497051789705E-11, -1.000000000000000000, 2.220446048198130405E-15 ) ) ;
#10541 = ORIENTED_EDGE ( 'NONE', *, *, #10691, .F. ) ;
#10542 = AXIS2_PLACEMENT_3D ( 'NONE', #18299, #10838, #1770 ) ;
#10543 = DIRECTION ( 'NONE',  ( 0.9999862922474492821, 0.005235963827122071951, -1.187304881134280213E-16 ) ) ;
#10544 = DIRECTION ( 'NONE',  ( -2.656137997592320068E-16, 6.783012436524469908E-17, 1.000000000000000000 ) ) ;
#10545 = ORIENTED_EDGE ( 'NONE', *, *, #10796, .F. ) ;
#10546 = VECTOR ( 'NONE', #9083, 1000.000000000000000 ) ;
#10547 = ADVANCED_FACE ( 'NONE', ( #9209 ), #45, .T. ) ;
#10548 = TOROIDAL_SURFACE ( 'NONE', #9396, 2.700000000000000178, 0.2000000000000000111 ) ;
#10549 = CONTEXT_DEPENDENT_SHAPE_REPRESENTATION ( #11850, #6687 ) ;
#10550 = FACE_OUTER_BOUND ( 'NONE', #22804, .T. ) ;
#10551 = VECTOR ( 'NONE', #6678, 999.9999999999998863 ) ;
#10552 = VERTEX_POINT ( 'NONE', #2188 ) ;
#10553 = ORIENTED_EDGE ( 'NONE', *, *, #9827, .F. ) ;
#10555 = COORDINATED_UNIVERSAL_TIME_OFFSET ( 0, 0, .AHEAD. ) ;
#10554 = PRODUCT_DEFINITION ( 'UNKNOWN', '', #14534, #17536 ) ;
#10556 = ORIENTED_EDGE ( 'NONE', *, *, #11595, .F. ) ;
#10557 = APPROVAL ( #3766, 'UNSPECIFIED' ) ;
#10558 = DIRECTION ( 'NONE',  ( -2.982858504577314686E-17, 2.441916418604790135E-15, 1.000000000000000000 ) ) ;
#10559 = PERSON_AND_ORGANIZATION_ROLE ( 'creator' ) ;
#10560 = AXIS2_PLACEMENT_3D ( 'NONE', #10799, #18022, #1491 ) ;
#10561 = ADVANCED_FACE ( 'NONE', ( #18363 ), #21788, .F. ) ;
#10562 = EDGE_CURVE ( 'NONE', #15552, #2375, #9443, .T. ) ;
#10563 = ADVANCED_FACE ( 'NONE', ( #5523 ), #395, .T. ) ;
#10564 = ITEM_DEFINED_TRANSFORMATION ( 'NONE', 'NONE', #13664,  #12739 ) ;
#10565 = VECTOR ( 'NONE', #15384, 1000.000000000000000 ) ;
#10566 = CARTESIAN_POINT ( 'NONE',  ( 122.7747609327790030, 11.20643158045800014, -9.133960000000000079 ) ) ;
#10567 = EDGE_CURVE ( 'NONE', #11059, #14140, #9146, .T. ) ;
#10568 = AXIS2_PLACEMENT_3D ( 'NONE', #20710, #18831, #522 ) ;
#10569 = CIRCLE ( 'NONE', #20784, 2.067000000000000615 ) ;
#10570 = CARTESIAN_POINT ( 'NONE',  ( 117.1241794131700118, -12.63305097454420078, -15.50000000000000000 ) ) ;
#10571 = ORIENTED_EDGE ( 'NONE', *, *, #8080, .F. ) ;
#10572 = ORIENTED_EDGE ( 'NONE', *, *, #4988, .F. ) ;
#10573 = LINE ( 'NONE', #23472, #13337 ) ;
#10574 = DIRECTION ( 'NONE',  ( -1.138590270679730064E-14, -2.220446049251240387E-15, -1.000000000000000000 ) ) ;
#10575 = ORIENTED_EDGE ( 'NONE', *, *, #9723, .F. ) ;
#10576 = EDGE_CURVE ( 'NONE', #3272, #2287, #15590, .T. ) ;
#10577 = DIRECTION ( 'NONE',  ( -0.9999862922474491711, -0.005235963827128302210, 1.187304881134281446E-16 ) ) ;
#10578 = DIRECTION ( 'NONE',  ( 3.210834492194344756E-17, -2.441916418604790135E-15, -1.000000000000000000 ) ) ;
#10579 = AXIS2_PLACEMENT_3D ( 'NONE', #2610, #2127, #20538 ) ;
#10580 = ORIENTED_EDGE ( 'NONE', *, *, #3498, .T. ) ;
#10581 = ORIENTED_EDGE ( 'NONE', *, *, #9317, .T. ) ;
#10582 = DATE_AND_TIME ( #1640, #14826 ) ;
#10583 = VERTEX_POINT ( 'NONE', #7780 ) ;
#10584 = ORIENTED_EDGE ( 'NONE', *, *, #4438, .F. ) ;
#10585 = LINE ( 'NONE', #1519, #11526 ) ;
#10586 = AXIS2_PLACEMENT_3D ( 'NONE', #12744, #8945, #12633 ) ;
#10587 = COORDINATED_UNIVERSAL_TIME_OFFSET ( 0, 0, .AHEAD. ) ;
#10588 = EDGE_CURVE ( 'NONE', #14947, #11330, #17493, .T. ) ;
#10589 = EDGE_CURVE ( 'NONE', #12554, #18732, #14454, .T. ) ;
#10590 = DIRECTION ( 'NONE',  ( -0.9999862922474492821, -0.005235963827121953122, 1.466966272682004590E-16 ) ) ;
#10591 = APPROVAL_DATE_TIME ( #17937, #8513 ) ;
#10592 = CARTESIAN_POINT ( 'NONE',  ( -12.59661859122890171, -1.225550774622830019, 5.500000000004429346 ) ) ;
#10593 = APPROVAL_DATE_TIME ( #5464, #6205 ) ;
#10594 = CLOSED_SHELL ( 'NONE', ( #10460, #20119, #20248, #10020, #4156, #1206 ) ) ;
#10595 = AXIS2_PLACEMENT_3D ( 'NONE', #8211, #13666, #1182 ) ;
#10596 = ORIENTED_EDGE ( 'NONE', *, *, #7741, .T. ) ;
#10597 = DIRECTION ( 'NONE',  ( 0.000000000000000000, 0.000000000000000000, -1.000000000000000000 ) ) ;
#10598 = FACE_OUTER_BOUND ( 'NONE', #584, .T. ) ;
#10599 = VERTEX_POINT ( 'NONE', #10054 ) ;
#10600 = ADVANCED_FACE ( 'NONE', ( #16800 ), #634, .T. ) ;
#10601 = CARTESIAN_POINT ( 'NONE',  ( 122.4288069621910040, 9.746871424029221131, -10.02499999999999858 ) ) ;
#10602 = DIRECTION ( 'NONE',  ( -1.187319687680494078E-16, -2.805478249478345354E-20, -1.000000000000000000 ) ) ;
#10603 = CARTESIAN_POINT ( 'NONE',  ( 118.4388045014059969, -7.086722380115170417, -18.89999999999999858 ) ) ;
#10604 = EDGE_LOOP ( 'NONE', ( #22669, #11011, #18486, #6287 ) ) ;
#10605 = EDGE_LOOP ( 'NONE', ( #3512, #2250, #19951, #23049 ) ) ;
#10607 = CARTESIAN_POINT ( 'NONE',  ( -16.50000000202540207, 1.899127378699210000, 5.500000000004470202 ) ) ;
#10606 = VECTOR ( 'NONE', #7553, 1000.000000000000000 ) ;
#10608 = PERSON_AND_ORGANIZATION_ROLE ( 'classification_officer' ) ;
#10609 = ORIENTED_EDGE ( 'NONE', *, *, #18167, .F. ) ;
#10610 = ORIENTED_EDGE ( 'NONE', *, *, #9977, .T. ) ;
#10611 = DIRECTION ( 'NONE',  ( 0.005235963827117092427, -0.9999862922474493931, -2.636227439667000721E-16 ) ) ;
#10612 = PLANE ( 'NONE',  #12132 ) ;
#10613 = ADVANCED_FACE ( 'NONE', ( #6239, #5993 ), #11718, .T. ) ;
#10614 = LINE ( 'NONE', #16055, #17893 ) ;
#10615 = PERSON_AND_ORGANIZATION_ROLE ( 'creator' ) ;
#10616 = EDGE_CURVE ( 'NONE', #1110, #17907, #16913, .T. ) ;
#10617 = CARTESIAN_POINT ( 'NONE',  ( 52.49909637502329929, -7.592283011512620305, -10.74538000000039872 ) ) ;
#10618 = CARTESIAN_POINT ( 'NONE',  ( -25.64168762722610140, 6.365828311191170208, -2.500000000000000000 ) ) ;
#10619 = CARTESIAN_POINT ( 'NONE',  ( 0.000000000000000000, 0.000000000000000000, 0.000000000000000000 ) ) ;
#10620 = SECURITY_CLASSIFICATION ( '', '', #793 ) ;
#10621 = VECTOR ( 'NONE', #7179, 1000.000000000000000 ) ;
#10622 = DIRECTION ( 'NONE',  ( -0.9730401042858024541, 0.2306359803922080898, 5.959266323858952312E-17 ) ) ;
#10623 = DATE_AND_TIME ( #8711, #18647 ) ;
#10624 = CARTESIAN_POINT ( 'NONE',  ( -20.00000000397360012, 22.95208919256889857, -3.750000000000000000 ) ) ;
#10625 = CARTESIAN_POINT ( 'NONE',  ( 31.01827548281339020, -2.500766059351137827, -15.00000000000039435 ) ) ;
#10626 = CARTESIAN_POINT ( 'NONE',  ( -3.458317987535628912, 19.03127855354509990, -5.000000000000000888 ) ) ;
#10627 = CARTESIAN_POINT ( 'NONE',  ( -25.29411765129449918, 25.77561860384869874, -7.999999999994368949 ) ) ;
#10628 = CARTESIAN_POINT ( 'NONE',  ( 33.90884364377009774, 10.17428291754599989, -29.25000000000050093 ) ) ;
#10629 = EDGE_LOOP ( 'NONE', ( #23112, #9757, #4289, #13210 ) ) ;
#10630 = CARTESIAN_POINT ( 'NONE',  ( 0.4338424296054549933, 18.10873463197630073, -7.340748883243850692E-15 ) ) ;
#10631 = UNCERTAINTY_MEASURE_WITH_UNIT (LENGTH_MEASURE( 1.000000000000000082E-05 ), #237, 'distance_accuracy_value', 'NONE');
#10632 = CC_DESIGN_DATE_AND_TIME_ASSIGNMENT ( #518, #9319, ( #1155 ) ) ;
#10633 = PRODUCT ( '1602p_c_19', '1602p_c_19', '', ( #6440 ) ) ;
#10634 = ORIENTED_EDGE ( 'NONE', *, *, #22107, .T. ) ;
#10635 = DIRECTION ( 'NONE',  ( -9.249330715586770885E-11, 1.000000000000000000, -2.220446028256680454E-15 ) ) ;
#10636 = CARTESIAN_POINT ( 'NONE',  ( -11.24263882182209962, 20.87636639668270178, -2.982050098520939832E-15 ) ) ;
#10637 = VECTOR ( 'NONE', #21076, 1000.000000000000000 ) ;
#10638 = ORIENTED_EDGE ( 'NONE', *, *, #2599, .F. ) ;
#10639 = AXIS2_PLACEMENT_3D ( 'NONE', #1667, #1895, #8929 ) ;
#10640 = DIRECTION ( 'NONE',  ( -1.000000000000000000, 0.000000000000000000, -1.749697687229200179E-14 ) ) ;
#10641 = ORIENTED_EDGE ( 'NONE', *, *, #12359, .T. ) ;
#10642 = FACE_OUTER_BOUND ( 'NONE', #13266, .T. ) ;
#10643 = COORDINATED_UNIVERSAL_TIME_OFFSET ( 0, 0, .AHEAD. ) ;
#10644 = CARTESIAN_POINT ( 'NONE',  ( 34.41917370704145185, 26.49663125198719982, -20.00000000000029843 ) ) ;
#10645 = VECTOR ( 'NONE', #4791, 1000.000000000000114 ) ;
#10646 = DIRECTION ( 'NONE',  ( 0.9730401042858035643, -0.2306359803922028717, -5.959266323858677443E-17 ) ) ;
#10647 = EDGE_CURVE ( 'NONE', #15489, #6052, #19062, .T. ) ;
#10648 = CYLINDRICAL_SURFACE ( 'NONE', #21151, 2.066999999999999726 ) ;
#10649 = DIRECTION ( 'NONE',  ( 1.000000000000000000, 0.000000000000000000, 0.000000000000000000 ) ) ;
#10650 = APPROVAL_PERSON_ORGANIZATION ( #13419, #18236, #4385 ) ;
#10651 = AXIS2_PLACEMENT_3D ( 'NONE', #4707, #2813, #10071 ) ;
#10652 = CARTESIAN_POINT ( 'NONE',  ( 30.72899802076640086, 10.92798958341530025, -1.881607274541729715E-15 ) ) ;
#10653 = VECTOR ( 'NONE', #5642, 1000.000000000000000 ) ;
#10654 = DIRECTION ( 'NONE',  ( -1.187319687680494078E-16, -2.805478249478260493E-20, -1.000000000000000000 ) ) ;
#10655 = DESIGN_CONTEXT ( 'detailed design', #9637, 'design' ) ;
#10656 = CARTESIAN_POINT ( 'NONE',  ( 2.499999999999987566, -17.30000000000000782, 2.500000000000000000 ) ) ;
#10657 = VERTEX_POINT ( 'NONE', #11485 ) ;
#10658 = CARTESIAN_POINT ( 'NONE',  ( -25.44812980900369936, 25.46511081327010118, 4.999999999999940492 ) ) ;
#10659 = DIRECTION ( 'NONE',  ( -0.2306359803922027885, -0.9730401042858034533, 4.741332172908048425E-18 ) ) ;
#10660 = EDGE_CURVE ( 'NONE', #20805, #13906, #7657, .T. ) ;
#10661 = EDGE_CURVE ( 'NONE', #14490, #1632, #9923, .T. ) ;
#10662 = ORIENTED_EDGE ( 'NONE', *, *, #4934, .T. ) ;
#10663 = DIRECTION ( 'NONE',  ( 3.837966487416234409E-32, -1.216195237911450118E-15, -1.000000000000000000 ) ) ;
#10664 = AXIS2_PLACEMENT_3D ( 'NONE', #8004, #15238, #8348 ) ;
#10665 = EDGE_LOOP ( 'NONE', ( #13184, #15956 ) ) ;
#10666 = EDGE_LOOP ( 'NONE', ( #5734, #12988, #17964, #14723 ) ) ;
#10667 = APPLICATION_CONTEXT ( 'configuration controlled 3d designs of mechanical parts and assemblies' ) ;
#10668 = APPROVAL_DATE_TIME ( #23341, #3134 ) ;
#10669 = FACE_BOUND ( 'NONE', #2601, .T. ) ;
#10670 = ORIENTED_EDGE ( 'NONE', *, *, #10067, .T. ) ;
#10671 = LOCAL_TIME ( 14, 11, 27.00000000000000000, #14502 ) ;
#10672 = DIRECTION ( 'NONE',  ( 0.000000000000000000, 1.000000000000000000, 0.000000000000000000 ) ) ;
#10673 = APPROVAL_PERSON_ORGANIZATION ( #3311, #6483, #14699 ) ;
#10674 = APPROVAL_DATE_TIME ( #9103, #23135 ) ;
#10675 = APPROVAL_STATUS ( 'not_yet_approved' ) ;
#10676 = DIRECTION ( 'NONE',  ( 0.005235963827110373843, -0.9999862922474493931, 0.000000000000000000 ) ) ;
#10677 = AXIS2_PLACEMENT_3D ( 'NONE', #11795, #19027, #3216 ) ;
#10678 = EDGE_CURVE ( 'NONE', #3314, #22720, #15251, .T. ) ;
#10679 = CARTESIAN_POINT ( 'NONE',  ( 0.000000000000000000, 0.000000000000000000, -5.000000000000000000 ) ) ;
#10680 = ORIENTED_EDGE ( 'NONE', *, *, #2327, .F. ) ;
#10681 = DIRECTION ( 'NONE',  ( -6.123237831918669245E-17, 0.000000000000000000, 1.000000000000000000 ) ) ;
#10682 = CC_DESIGN_PERSON_AND_ORGANIZATION_ASSIGNMENT ( #2293, #14654, ( #17596 ) ) ;
#10683 = SECURITY_CLASSIFICATION ( '', '', #14355 ) ;
#10684 = APPROVAL ( #1677, 'UNSPECIFIED' ) ;
#10685 = VERTEX_POINT ( 'NONE', #4211 ) ;
#10686 = LOCAL_TIME ( 14, 11, 27.00000000000000000, #4173 ) ;
#10687 = DIRECTION ( 'NONE',  ( -0.9999862922474492821, -0.005235963827121822151, 1.466966272681990292E-16 ) ) ;
#10688 = CARTESIAN_POINT ( 'NONE',  ( -4.514225866272970400, 4.676725866273559795, -2.500000000000000000 ) ) ;
#10689 = EDGE_LOOP ( 'NONE', ( #19754, #3190, #13460, #17331, #16873 ) ) ;
#10690 = EDGE_CURVE ( 'NONE', #815, #9785, #13127, .T. ) ;
#10691 = EDGE_CURVE ( 'NONE', #4833, #7064, #20363, .T. ) ;
#10692 = ORGANIZATION ( 'NAUO-ORG41', 'UNSPECIFIED', 'UNSPECIFIED' ) ;
#10693 = CARTESIAN_POINT ( 'NONE',  ( 43.87899317387989839, 21.17128575569940097, 13.00000000000000000 ) ) ;
#10694 = CARTESIAN_POINT ( 'NONE',  ( -22.52506283708579815, 28.95208917575130414, 5.500000000004479972 ) ) ;
#10695 = ORIENTED_EDGE ( 'NONE', *, *, #20154, .F. ) ;
#10696 = LOCAL_TIME ( 14, 11, 27.00000000000000000, #1494 ) ;
#10697 = ORIENTED_EDGE ( 'NONE', *, *, #17837, .F. ) ;
#10698 = COORDINATED_UNIVERSAL_TIME_OFFSET ( 0, 0, .AHEAD. ) ;
#10699 = ADVANCED_FACE ( 'NONE', ( #2442 ), #13360, .T. ) ;
#10700 = ORIENTED_EDGE ( 'NONE', *, *, #21508, .T. ) ;
#10701 = ORIENTED_EDGE ( 'NONE', *, *, #13299, .F. ) ;
#10702 = DIRECTION ( 'NONE',  ( -0.07397971354964476276, -0.9972597464969256142, 2.428612866367529538E-15 ) ) ;
#10703 = PERSON_AND_ORGANIZATION_ROLE ( 'creator' ) ;
#10704 = CC_DESIGN_SECURITY_CLASSIFICATION ( #9559, ( #14088 ) ) ;
#10705 = CARTESIAN_POINT ( 'NONE',  ( -3.499952022866071211, -0.01832587339492825623, 8.925353670776949322E-14 ) ) ;
#10706 = COORDINATED_UNIVERSAL_TIME_OFFSET ( 0, 0, .AHEAD. ) ;
#10707 = CIRCLE ( 'NONE', #16746, 3.499999999999998224 ) ;
#10708 = EDGE_CURVE ( 'NONE', #9363, #20644, #15977, .T. ) ;
#10709 = LOCAL_TIME ( 14, 11, 27.00000000000000000, #20967 ) ;
#10710 = DIRECTION ( 'NONE',  ( 0.9999862922474493931, 0.005235963827108232327, -1.922962686383570719E-16 ) ) ;
#10711 = PRODUCT_DEFINITION ( 'UNKNOWN', '', #1599, #13735 ) ;
#10712 = COORDINATED_UNIVERSAL_TIME_OFFSET ( 0, 0, .AHEAD. ) ;
#10713 = APPROVAL ( #939, 'UNSPECIFIED' ) ;
#10714 = ORIENTED_EDGE ( 'NONE', *, *, #22896, .T. ) ;
#10715 = FACE_BOUND ( 'NONE', #12893, .T. ) ;
#10716 = FACE_OUTER_BOUND ( 'NONE', #13164, .T. ) ;
#10717 = ORIENTED_EDGE ( 'NONE', *, *, #752, .F. ) ;
#10718 = EDGE_CURVE ( 'NONE', #19011, #21767, #11362, .T. ) ;
#10719 = EDGE_CURVE ( 'NONE', #13532, #13022, #22352, .T. ) ;
#10720 = CC_DESIGN_SECURITY_CLASSIFICATION ( #11475, ( #795 ) ) ;
#10721 = LINE ( 'NONE', #16267, #6353 ) ;
#10722 = CARTESIAN_POINT ( 'NONE',  ( 0.000000000000000000, -17.30000000000000071, -2.500000000000000000 ) ) ;
#10723 = CARTESIAN_POINT ( 'NONE',  ( 39.67523673029199927, 5.313293424921989860, 18.89999999999999858 ) ) ;
#10724 = EDGE_LOOP ( 'NONE', ( #1045, #8646, #5683, #16277, #4280 ) ) ;
#10725 = EDGE_LOOP ( 'NONE', ( #3361, #2194, #12155, #19449 ) ) ;
#10726 = CYLINDRICAL_SURFACE ( 'NONE', #10639, 2.066999999999999726 ) ;
#10727 = VECTOR ( 'NONE', #20285, 1000.000000000000114 ) ;
#10728 = VERTEX_POINT ( 'NONE', #4446 ) ;
#10729 = DATE_TIME_ROLE ( 'creation_date' ) ;
#10730 = ORIENTED_EDGE ( 'NONE', *, *, #17072, .T. ) ;
#10731 = ORIENTED_EDGE ( 'NONE', *, *, #8656, .F. ) ;
#10732 = DIRECTION ( 'NONE',  ( -0.9730401042858035643, 0.2306359803922028717, 5.667427308550587516E-17 ) ) ;
#10733 = AXIS2_PLACEMENT_3D ( 'NONE', #22877, #15637, #6740 ) ;
#10734 = CARTESIAN_POINT ( 'NONE',  ( -2.500000000000012434, -17.29999999999999361, 2.500000000000000000 ) ) ;
#10735 = SECURITY_CLASSIFICATION ( '', '', #11040 ) ;
#10736 = FACE_OUTER_BOUND ( 'NONE', #13269, .T. ) ;
#10737 = COORDINATED_UNIVERSAL_TIME_OFFSET ( 0, 0, .AHEAD. ) ;
#10738 = DIRECTION ( 'NONE',  ( 0.2306359803922080898, 0.9730401042858024541, -2.572202231434325988E-16 ) ) ;
#10739 = FACE_OUTER_BOUND ( 'NONE', #7329, .T. ) ;
#10740 = AXIS2_PLACEMENT_3D ( 'NONE', #10475, #4755, #21374 ) ;
#10741 = EDGE_CURVE ( 'NONE', #15256, #1296, #21415, .T. ) ;
#10742 = APPROVAL_PERSON_ORGANIZATION ( #5559, #7933, #21589 ) ;
#10743 = CARTESIAN_POINT ( 'NONE',  ( 0.000000000000000000, 0.000000000000000000, 0.000000000000000000 ) ) ;
#10744 = CIRCLE ( 'NONE', #12632, 2.500000000000000888 ) ;
#10745 = AXIS2_PLACEMENT_3D ( 'NONE', #15373, #11491, #7786 ) ;
#10746 = PLANE ( 'NONE',  #15098 ) ;
#10747 = APPROVAL_STATUS ( 'not_yet_approved' ) ;
#10748 = CIRCLE ( 'NONE', #11118, 2.500000000000000000 ) ;
#10749 = CARTESIAN_POINT ( 'NONE',  ( -26.99999999999959854, -19.33065833018799751, 23.00000000000000000 ) ) ;
#10750 = CARTESIAN_POINT ( 'NONE',  ( 28.03349347434003747, -5.647195339844054196, -13.00000000000039968 ) ) ;
#10751 = ADVANCED_FACE ( 'NONE', ( #6709 ), #21175, .T. ) ;
#10752 = AXIS2_PLACEMENT_3D ( 'NONE', #2793, #4214, #5996 ) ;
#10753 = FACE_OUTER_BOUND ( 'NONE', #8766, .T. ) ;
#10754 = DIRECTION ( 'NONE',  ( 0.2306359803922021778, 0.9730401042858037863, -1.407521210652540770E-17 ) ) ;
#10755 = ADVANCED_FACE ( 'NONE', ( #15839 ), #1499, .T. ) ;
#10756 = FACE_OUTER_BOUND ( 'NONE', #8884, .T. ) ;
#10757 = ORIENTED_EDGE ( 'NONE', *, *, #16938, .F. ) ;
#10758 = AXIS2_PLACEMENT_3D ( 'NONE', #13171, #9738, #20408 ) ;
#10759 = CARTESIAN_POINT ( 'NONE',  ( 112.6956120935907251, 3.369770385951719849, 2.067000000000031701 ) ) ;
#10760 = VECTOR ( 'NONE', #207, 1000.000000000000227 ) ;
#10761 = LOCAL_TIME ( 14, 11, 27.00000000000000000, #890 ) ;
#10762 = EDGE_LOOP ( 'NONE', ( #6676, #19466, #17054, #8674 ) ) ;
#10763 = FACE_OUTER_BOUND ( 'NONE', #11574, .T. ) ;
#10764 = DIRECTION ( 'NONE',  ( 0.000000000000000000, 0.000000000000000000, -1.000000000000000000 ) ) ;
#10765 = ORIENTED_EDGE ( 'NONE', *, *, #22601, .T. ) ;
#10766 = CIRCLE ( 'NONE', #10003, 5.000000000000001776 ) ;
#10767 = TOROIDAL_SURFACE ( 'NONE', #20215, 2.380000000000000338, 2.370000000000000107 ) ;
#10768 = FACE_OUTER_BOUND ( 'NONE', #2055, .T. ) ;
#10769 = EDGE_LOOP ( 'NONE', ( #20197, #4650 ) ) ;
#10770 = VECTOR ( 'NONE', #9909, 1000.000000000000227 ) ;
#10771 = DIRECTION ( 'NONE',  ( -0.2306359803922028995, -0.9730401042858035643, 3.648592655857288816E-32 ) ) ;
#10772 = CALENDAR_DATE ( 2026, 31, 10 ) ;
#10773 = FACE_OUTER_BOUND ( 'NONE', #17667, .T. ) ;
#10774 = CIRCLE ( 'NONE', #1265, 3.750000000000000000 ) ;
#10775 = CARTESIAN_POINT ( 'NONE',  ( -6.610902845792273830, 17.65425360406484856, -1.280106301620261415E-15 ) ) ;
#10776 = CC_DESIGN_DATE_AND_TIME_ASSIGNMENT ( #6420, #17465, ( #3051 ) ) ;
#10777 = DIRECTION ( 'NONE',  ( -0.9730401042858024541, 0.2306359803922080898, 5.959266323858723049E-17 ) ) ;
#10778 = APPROVAL_ROLE ( '' ) ;
#10779 = APPROVAL_PERSON_ORGANIZATION ( #13348, #12001, #6094 ) ;
#10780 = EDGE_CURVE ( 'NONE', #813, #10964, #19633, .T. ) ;
#10781 = VECTOR ( 'NONE', #22869, 1000.000000000000114 ) ;
#10782 = DIRECTION ( 'NONE',  ( 5.899155740360660338E-30, 4.861311874477930828E-15, 1.000000000000000000 ) ) ;
#10783 = AXIS2_PLACEMENT_3D ( 'NONE', #9090, #11006, #18013 ) ;
#10784 = CYLINDRICAL_SURFACE ( 'NONE', #15850, 6.000000000000000000 ) ;
#10785 = FACE_OUTER_BOUND ( 'NONE', #7175, .T. ) ;
#10786 = AXIS2_PLACEMENT_3D ( 'NONE', #8286, #908, #15517 ) ;
#10787 = CARTESIAN_POINT ( 'NONE',  ( 5.000000000000000000, -23.36217782649100272, -2.500000000000000000 ) ) ;
#10788 = ORIENTED_EDGE ( 'NONE', *, *, #7913, .F. ) ;
#10789 = DIRECTION ( 'NONE',  ( -1.751019220569994795E-16, -2.300154215587015208E-15, -1.000000000000000000 ) ) ;
#10790 = CARTESIAN_POINT ( 'NONE',  ( 105.1303954406765939, 6.139246328161051203, 3.645906919371072791E-14 ) ) ;
#10791 = ORIENTED_EDGE ( 'NONE', *, *, #14071, .F. ) ;
#10792 = CARTESIAN_POINT ( 'NONE',  ( -20.00000000397090005, 22.95208919256900160, 8.000000000004460432 ) ) ;
#10793 = VERTEX_POINT ( 'NONE', #1452 ) ;
#10794 = DATE_TIME_ROLE ( 'classification_date' ) ;
#10795 = DIRECTION ( 'NONE',  ( 0.000000000000000000, 0.000000000000000000, -1.000000000000000000 ) ) ;
#10796 = EDGE_CURVE ( 'NONE', #16722, #1889, #11784, .T. ) ;
#10797 = VECTOR ( 'NONE', #3623, 1000.000000000000000 ) ;
#10798 = ORIENTED_EDGE ( 'NONE', *, *, #23202, .F. ) ;
#10799 = CARTESIAN_POINT ( 'NONE',  ( -19.49999999982360066, -0.1021026942259749964, -2.500000000000000000 ) ) ;
#10800 = SHAPE_DEFINITION_REPRESENTATION ( #20879, #7037 ) ;
#10801 = PERSON_AND_ORGANIZATION_ROLE ( 'classification_officer' ) ;
#10802 = CARTESIAN_POINT ( 'NONE',  ( -25.29411765129259848, 25.77561860384869874, 5.500000000004519940 ) ) ;
#10803 = CARTESIAN_POINT ( 'NONE',  ( 122.7747609327790030, 11.20643158045800014, -9.133960000000000079 ) ) ;
#10804 = VERTEX_POINT ( 'NONE', #17747 ) ;
#10805 = PERSON ( 'NAUO-PER23', 'UNSPECIFIED', 'UNSPECIFIED', ('UNSPECIFIED'), ('UNSPECIFIED'), ('UNSPECIFIED') ) ;
#10806 = DIRECTION ( 'NONE',  ( 1.000000000000000000, -5.913983195221379736E-15, 0.000000000000000000 ) ) ;
#10807 = VERTEX_POINT ( 'NONE', #10164 ) ;
#10808 = DIRECTION ( 'NONE',  ( 3.210834492194344756E-17, -2.441916418604790135E-15, -1.000000000000000000 ) ) ;
#10809 = CARTESIAN_POINT ( 'NONE',  ( -62.91413607658799378, 7.983193290926554830, 2.458500000000002572 ) ) ;
#10810 = CARTESIAN_POINT ( 'NONE',  ( -65.64475015647069256, -21.84411297095480009, 5.000000000000000000 ) ) ;
#10811 = ORIENTED_EDGE ( 'NONE', *, *, #17901, .T. ) ;
#10812 = CARTESIAN_POINT ( 'NONE',  ( 28.89837840081079534, -1.998294948772295410, -17.25000000000040146 ) ) ;
#10813 = DIRECTION ( 'NONE',  ( -0.2867834340965239592, 0.9579954394086668268, -4.742590440343770138E-15 ) ) ;
#10814 = ORIENTED_EDGE ( 'NONE', *, *, #11446, .T. ) ;
#10815 = DATE_AND_TIME ( #3555, #8769 ) ;
#10816 = ADVANCED_FACE ( 'NONE', ( #3359 ), #15924, .T. ) ;
#10817 = ORIENTED_EDGE ( 'NONE', *, *, #19963, .T. ) ;
#10818 = ORIENTED_EDGE ( 'NONE', *, *, #7777, .T. ) ;
#10819 = CARTESIAN_POINT ( 'NONE',  ( -0.5391976746803449627, 18.33937061236850141, -7.621247264287879719E-15 ) ) ;
#10820 = APPROVAL_DATE_TIME ( #16138, #19836 ) ;
#10821 = APPROVAL ( #5776, 'UNKNOWN' ) ;
#10822 = ADVANCED_BREP_SHAPE_REPRESENTATION ( '', ( #17344, #12739 ), #19347 ) ;
#10823 = CARTESIAN_POINT ( 'NONE',  ( 6.500000000000000000, -17.30000000000000071, 2.500000000000000000 ) ) ;
#10824 = SECURITY_CLASSIFICATION_LEVEL ( 'unclassified' ) ;
#10825 = CARTESIAN_POINT ( 'NONE',  ( 34.67470932959370344, 24.53963568513860238, -15.00000000000049916 ) ) ;
#10826 = ADVANCED_FACE ( 'NONE', ( #10407 ), #15950, .F. ) ;
#10827 = ADVANCED_FACE ( 'NONE', ( #12180 ), #19404, .F. ) ;
#10828 = CIRCLE ( 'NONE', #6649, 0.3999999999999982458 ) ;
#10829 = DIRECTION ( 'NONE',  ( -0.9730401042858024541, 0.2306359803922080898, 5.959266323858942451E-17 ) ) ;
#10830 = EDGE_CURVE ( 'NONE', #20796, #9360, #12416, .T. ) ;
#10831 = PERSON_AND_ORGANIZATION ( #11966, #8758 ) ;
#10832 = PRODUCT ( '1602p_c_43', '1602p_c_43', '', ( #13667 ) ) ;
#10833 = EDGE_CURVE ( 'NONE', #9640, #2031, #4825, .T. ) ;
#10834 = ORIENTED_EDGE ( 'NONE', *, *, #7055, .F. ) ;
#10835 = CARTESIAN_POINT ( 'NONE',  ( 35.94015251278350576, 11.23436983788199761, -27.55602540378494325 ) ) ;
#10836 = CARTESIAN_POINT ( 'NONE',  ( 35.01760859121468172, 7.342209420738994297, 17.70000000000000995 ) ) ;
#10837 = VERTEX_POINT ( 'NONE', #10627 ) ;
#10838 = DIRECTION ( 'NONE',  ( 0.9730401042858036753, -0.2306359803922031493, -5.432877459303553216E-17 ) ) ;
#10839 = AXIS2_PLACEMENT_3D ( 'NONE', #11758, #16716, #7825 ) ;
#10840 = CARTESIAN_POINT ( 'NONE',  ( 35.11747397072451804, 7.763535785894483787, -37.44562646538079065 ) ) ;
#10841 = CARTESIAN_POINT ( 'NONE',  ( 2.499999999999970246, -31.09999999999999787, 19.00000000000000000 ) ) ;
#10842 = ORIENTED_EDGE ( 'NONE', *, *, #15496, .F. ) ;
#10843 = EDGE_LOOP ( 'NONE', ( #5437, #14475, #16667 ) ) ;
#10844 = DIRECTION ( 'NONE',  ( -0.9730401042858024541, 0.2306359803922080898, 5.959266323858942451E-17 ) ) ;
#10845 = ORIENTED_EDGE ( 'NONE', *, *, #13013, .T. ) ;
#10846 = APPROVAL_STATUS ( 'not_yet_approved' ) ;
#10847 = ADVANCED_FACE ( 'NONE', ( #6594, #1335 ), #985, .F. ) ;
#10848 = VERTEX_POINT ( 'NONE', #12402 ) ;
#10849 = ORIENTED_EDGE ( 'NONE', *, *, #20558, .T. ) ;
#10850 = CARTESIAN_POINT ( 'NONE',  ( -28.52462712253550237, 6.350733138482030249, 0.7325259402521719920 ) ) ;
#10851 = LINE ( 'NONE', #1786, #21044 ) ;
#10852 = COORDINATED_UNIVERSAL_TIME_OFFSET ( 0, 0, .AHEAD. ) ;
#10853 = LINE ( 'NONE', #7161, #984 ) ;
#10854 = PRODUCT_DEFINITION ( 'UNKNOWN', '', #5427, #9207 ) ;
#10855 = APPROVAL ( #18399, 'UNSPECIFIED' ) ;
#10856 = DIRECTION ( 'NONE',  ( -0.9730401042858035643, 0.2306359803922028717, 5.958148513035547083E-17 ) ) ;
#10857 =( REPRESENTATION_RELATIONSHIP ('NONE','NONE', #18121, #2509 ) REPRESENTATION_RELATIONSHIP_WITH_TRANSFORMATION ( #9627 )SHAPE_REPRESENTATION_RELATIONSHIP( ) );
#10858 = EDGE_CURVE ( 'NONE', #23458, #9773, #16959, .T. ) ;
#10859 = EDGE_CURVE ( 'NONE', #8755, #21302, #10507, .T. ) ;
#10860 = AXIS2_PLACEMENT_3D ( 'NONE', #7798, #9716, #16566 ) ;
#10861 = CC_DESIGN_PERSON_AND_ORGANIZATION_ASSIGNMENT ( #8184, #15180, ( #16680 ) ) ;
#10862 = SHAPE_REPRESENTATION ( '1602p_c_44', ( #12739 ), #743 ) ;
#10863 = CARTESIAN_POINT ( 'NONE',  ( 0.000000000000000000, 0.000000000000000000, 0.000000000000000000 ) ) ;
#10864 = EDGE_CURVE ( 'NONE', #1889, #16722, #23024, .T. ) ;
#10865 = CIRCLE ( 'NONE', #19200, 2.066999999999997062 ) ;
#10866 = CARTESIAN_POINT ( 'NONE',  ( 0.5868595415223922807, -1.010778882616252483, -21.50000000000000000 ) ) ;
#10867 = APPROVAL_DATE_TIME ( #14275, #11056 ) ;
#10868 = DIRECTION ( 'NONE',  ( 0.2306359803922080343, 0.9730401042858022320, -2.572202231434325495E-16 ) ) ;
#10869 = DIRECTION ( 'NONE',  ( 6.052506032659479608E-17, 4.865024487662030352E-15, 1.000000000000000000 ) ) ;
#10870 = DIRECTION ( 'NONE',  ( -0.005225493778937319485, 0.9999863470141810984, 0.000000000000000000 ) ) ;
#10871 = DIRECTION ( 'NONE',  ( -0.9730401042858022320, 0.2306359803922080343, 5.959266323858941219E-17 ) ) ;
#10872 = DIRECTION ( 'NONE',  ( 0.2306359803922080898, 0.9730401042858024541, -2.572202231434325988E-16 ) ) ;
#10873 = VERTEX_POINT ( 'NONE', #13705 ) ;
#10874 = CARTESIAN_POINT ( 'NONE',  ( 34.28553241885766312, 11.38049369541048783, 8.912006346179969896 ) ) ;
#10875 = EDGE_CURVE ( 'NONE', #19270, #2029, #15724, .T. ) ;
#10876 = VERTEX_POINT ( 'NONE', #11094 ) ;
#10877 = CARTESIAN_POINT ( 'NONE',  ( 117.0319250210129951, -13.02226701625859917, 18.89999999999999858 ) ) ;
#10878 = DIRECTION ( 'NONE',  ( 0.000000000000000000, 0.000000000000000000, -1.000000000000000000 ) ) ;
#10879 = ORIENTED_EDGE ( 'NONE', *, *, #499, .T. ) ;
#10880 = CARTESIAN_POINT ( 'NONE',  ( -11.72915887396500167, 20.99168438687879856, -3.119098571846229552E-15 ) ) ;
#10881 = EDGE_CURVE ( 'NONE', #23172, #13198, #17778, .T. ) ;
#10882 = VECTOR ( 'NONE', #12370, 1000.000000000000114 ) ;
#10883 = ORIENTED_EDGE ( 'NONE', *, *, #8323, .F. ) ;
#10884 = DIRECTION ( 'NONE',  ( 0.2306359803922025109, 0.9730401042858035643, -5.112869192352692394E-15 ) ) ;
#10885 = PERSON_AND_ORGANIZATION ( #11966, #8758 ) ;
#10886 = CARTESIAN_POINT ( 'NONE',  ( 34.41917370704150159, 26.49663125198739877, 19.99999999999975131 ) ) ;
#10887 = EDGE_CURVE ( 'NONE', #15962, #8685, #16414, .T. ) ;
#10888 = PRODUCT_DEFINITION_SHAPE ( 'NONE', 'NONE',  #23514 ) ;
#10889 = EDGE_CURVE ( 'NONE', #18259, #23367, #20738, .T. ) ;
#10890 = FACE_OUTER_BOUND ( 'NONE', #6864, .T. ) ;
#10891 = DIRECTION ( 'NONE',  ( -1.000000000000000000, 0.000000000000000000, 0.000000000000000000 ) ) ;
#10892 = CARTESIAN_POINT ( 'NONE',  ( 0.000000000000000000, 0.000000000000000000, 0.000000000000000000 ) ) ;
#10893 = AXIS2_PLACEMENT_3D ( 'NONE', #5703, #12505, #11211 ) ;
#10894 = CIRCLE ( 'NONE', #14660, 2.500000000000000444 ) ;
#10895 = FACE_OUTER_BOUND ( 'NONE', #21427, .T. ) ;
#10896 = CARTESIAN_POINT ( 'NONE',  ( 40.45939906362439586, 8.621629779493279244, -2.477422125845284522E-15 ) ) ;
#10897 = CARTESIAN_POINT ( 'NONE',  ( 118.6002496876800052, -6.405594307115080710, -18.89999999999999858 ) ) ;
#10898 = DESIGN_CONTEXT ( 'detailed design', #22956, 'design' ) ;
#10899 = DIRECTION ( 'NONE',  ( -0.02168293463503252055, 0.9997648975362223300, -2.428612866367530721E-15 ) ) ;
#10900 = VERTEX_POINT ( 'NONE', #19879 ) ;
#10901 = CARTESIAN_POINT ( 'NONE',  ( 31.49419854219519976, 9.774809681453278998, 21.49999999999999289 ) ) ;
#10902 = DIRECTION ( 'NONE',  ( -7.691776389375310104E-16, -3.433811468266040107E-18, -1.000000000000000000 ) ) ;
#10903 = ORIENTED_EDGE ( 'NONE', *, *, #15197, .F. ) ;
#10904 = ORIENTED_EDGE ( 'NONE', *, *, #9792, .F. ) ;
#10905 = DIRECTION ( 'NONE',  ( 0.000000000000000000, -1.000000000000000000, 0.000000000000000000 ) ) ;
#10906 = CARTESIAN_POINT ( 'NONE',  ( 27.87922736721089834, -4.130116823143030302, -13.00000000000039968 ) ) ;
#10907 = ORIENTED_EDGE ( 'NONE', *, *, #18253, .F. ) ;
#10908 = DATE_TIME_ROLE ( 'creation_date' ) ;
#10909 = EDGE_CURVE ( 'NONE', #10449, #8039, #16183, .T. ) ;
#10910 = ORIENTED_EDGE ( 'NONE', *, *, #19429, .T. ) ;
#10911 = CIRCLE ( 'NONE', #12420, 12.49999999999999467 ) ;
#10912 = AXIS2_PLACEMENT_3D ( 'NONE', #21116, #19578, #7011 ) ;
#10913 = AXIS2_PLACEMENT_3D ( 'NONE', #17394, #3005, #1216 ) ;
#10914 = EDGE_CURVE ( 'NONE', #19758, #8608, #18331, .T. ) ;
#10915 = SECURITY_CLASSIFICATION_LEVEL ( 'unclassified' ) ;
#10916 = ADVANCED_FACE ( 'NONE', ( #8951 ), #5376, .T. ) ;
#10917 = DATE_AND_TIME ( #1971, #3846 ) ;
#10918 = CARTESIAN_POINT ( 'NONE',  ( -14.00000000202680006, 1.899127378930359988, -5.499999999996879829 ) ) ;
#10919 = VECTOR ( 'NONE', #10871, 1000.000000000000227 ) ;
#10920 = CARTESIAN_POINT ( 'NONE',  ( 31.49419854219519976, 9.774809681453278998, -21.50000000000000000 ) ) ;
#10921 = VERTEX_POINT ( 'NONE', #14640 ) ;
#10922 = DIRECTION ( 'NONE',  ( -1.918983243708115015E-32, 3.790318773197884981E-16, -1.000000000000000000 ) ) ;
#10923 = AXIS2_PLACEMENT_3D ( 'NONE', #5740, #11115, #12995 ) ;
#10924 = VECTOR ( 'NONE', #6555, 1000.000000000000000 ) ;
#10925 = EDGE_LOOP ( 'NONE', ( #3788, #13340 ) ) ;
#10926 = LINE ( 'NONE', #5659, #9749 ) ;
#10927 = FACE_OUTER_BOUND ( 'NONE', #3661, .T. ) ;
#10928 = DIRECTION ( 'NONE',  ( -0.9730401042858036753, 0.2306359803922031493, -2.740969466505752002E-16 ) ) ;
#10929 = ORIENTED_EDGE ( 'NONE', *, *, #11246, .T. ) ;
#10930 = COORDINATED_UNIVERSAL_TIME_OFFSET ( 0, 0, .AHEAD. ) ;
#10931 = CARTESIAN_POINT ( 'NONE',  ( 39.69419854219519550, 9.774809681453278998, -23.00000000000000000 ) ) ;
#10932 = AXIS2_PLACEMENT_3D ( 'NONE', #19169, #22586, #22699 ) ;
#10933 = EDGE_LOOP ( 'NONE', ( #19927, #6873, #11341, #15608, #3022, #6780, #21934, #22190 ) ) ;
#10934 = CALENDAR_DATE ( 2026, 31, 10 ) ;
#10935 = ORIENTED_EDGE ( 'NONE', *, *, #15033, .F. ) ;
#10936 = ORIENTED_EDGE ( 'NONE', *, *, #289, .F. ) ;
#10937 = CARTESIAN_POINT ( 'NONE',  ( -31.64160538070510142, 6.334412527122579739, -2.500000000000000000 ) ) ;
#10938 = AXIS2_PLACEMENT_3D ( 'NONE', #19495, #23039, #4528 ) ;
#10939 = COORDINATED_UNIVERSAL_TIME_OFFSET ( 0, 0, .AHEAD. ) ;
#10940 = DIRECTION ( 'NONE',  ( -0.2306359803922028995, -0.9730401042858035643, 3.648592655857288816E-32 ) ) ;
#10941 = ITEM_DEFINED_TRANSFORMATION ( 'NONE', 'NONE', #17069,  #12739 ) ;
#10942 = CIRCLE ( 'NONE', #16225, 3.500000000000000444 ) ;
#10943 = DIRECTION ( 'NONE',  ( -0.9730401042858035643, 0.2306359803922028717, 6.126766849694256332E-17 ) ) ;
#10944 = FACE_OUTER_BOUND ( 'NONE', #12964, .T. ) ;
#10945 = VECTOR ( 'NONE', #20376, 1000.000000000000227 ) ;
#10946 = EDGE_CURVE ( 'NONE', #12386, #19462, #8844, .T. ) ;
#10947 = EDGE_CURVE ( 'NONE', #10370, #22814, #4458, .T. ) ;
#10948 = COORDINATED_UNIVERSAL_TIME_OFFSET ( 0, 0, .AHEAD. ) ;
#10949 = EDGE_LOOP ( 'NONE', ( #17573, #14666, #2726, #9887 ) ) ;
#10950 = AXIS2_PLACEMENT_3D ( 'NONE', #12009, #19342, #19230 ) ;
#10951 = DIRECTION ( 'NONE',  ( 1.000000000000000000, -4.028143194477080210E-16, -1.401298464324815982E-46 ) ) ;
#10952 = EDGE_LOOP ( 'NONE', ( #11285, #8927, #12887, #5618 ) ) ;
#10953 = DIRECTION ( 'NONE',  ( -0.6944962871189153120, 0.7194962871190101472, 0.000000000000000000 ) ) ;
#10955 = VECTOR ( 'NONE', #2150, 1000.000000000000000 ) ;
#10954 = DIRECTION ( 'NONE',  ( 1.187319687680494078E-16, 2.805478249478345354E-20, 1.000000000000000000 ) ) ;
#10956 = FACE_OUTER_BOUND ( 'NONE', #10494, .T. ) ;
#10957 = EDGE_LOOP ( 'NONE', ( #12440, #14877, #12220, #16147, #22955 ) ) ;
#10958 = EDGE_LOOP ( 'NONE', ( #9408, #3865, #1626, #4425 ) ) ;
#10959 = LINE ( 'NONE', #9153, #4925 ) ;
#10960 = EDGE_LOOP ( 'NONE', ( #3660, #22470 ) ) ;
#10961 = EDGE_CURVE ( 'NONE', #886, #815, #13931, .T. ) ;
#10962 = EDGE_CURVE ( 'NONE', #21387, #16446, #7474, .T. ) ;
#10963 = APPROVAL_ROLE ( '' ) ;
#10964 = VERTEX_POINT ( 'NONE', #21870 ) ;
#10965 = EDGE_LOOP ( 'NONE', ( #22533, #12182, #10439, #10972, #21168 ) ) ;
#10966 = FACE_OUTER_BOUND ( 'NONE', #12922, .T. ) ;
#10967 = LINE ( 'NONE', #11433, #21796 ) ;
#10968 = DATE_TIME_ROLE ( 'classification_date' ) ;
#10969 = DIRECTION ( 'NONE',  ( 0.000000000000000000, 0.000000000000000000, 1.000000000000000000 ) ) ;
#10970 = DIRECTION ( 'NONE',  ( 0.1187863113461966047, 0.5011527021216413136, -0.8571673007021102242 ) ) ;
#10971 = CIRCLE ( 'NONE', #18928, 2.750000000000001776 ) ;
#10972 = ORIENTED_EDGE ( 'NONE', *, *, #9512, .F. ) ;
#10973 = DIRECTION ( 'NONE',  ( 0.9999862922474493931, 0.005235963827108152530, 0.000000000000000000 ) ) ;
#10974 = EDGE_CURVE ( 'NONE', #22662, #5508, #16556, .T. ) ;
#10975 = CALENDAR_DATE ( 2026, 31, 10 ) ;
#10976 = ORIENTED_EDGE ( 'NONE', *, *, #1217, .F. ) ;
#10977 = CARTESIAN_POINT ( 'NONE',  ( -24.86147400983239919, -14.96352599016710094, 2.500000000000000000 ) ) ;
#10978 = DIRECTION ( 'NONE',  ( 0.2306359803922080343, 0.9730401042858022320, 5.907067092757111157E-15 ) ) ;
#10979 = CC_DESIGN_DATE_AND_TIME_ASSIGNMENT ( #5562, #21939, ( #7962 ) ) ;
#10980 = FACE_BOUND ( 'NONE', #15628, .T. ) ;
#10981 = CC_DESIGN_DATE_AND_TIME_ASSIGNMENT ( #12842, #345, ( #19382 ) ) ;
#10982 = DIRECTION ( 'NONE',  ( -2.982858504577319616E-17, 2.441916418604790135E-15, 1.000000000000000000 ) ) ;
#10983 = ORIENTED_EDGE ( 'NONE', *, *, #7330, .F. ) ;
#10984 = CARTESIAN_POINT ( 'NONE',  ( 113.2033677465029911, -29.17473274740279976, -13.00000000000000000 ) ) ;
#10985 = EDGE_CURVE ( 'NONE', #13627, #8907, #5499, .T. ) ;
#10986 = EDGE_CURVE ( 'NONE', #21478, #20926, #16199, .T. ) ;
#10987 = ORIENTED_EDGE ( 'NONE', *, *, #2871, .F. ) ;
#10988 = LINE ( 'NONE', #18098, #16804 ) ;
#10989 = LINE ( 'NONE', #9307, #4525 ) ;
#10990 = ORIENTED_EDGE ( 'NONE', *, *, #10184, .F. ) ;
#10991 = DIRECTION ( 'NONE',  ( -0.9730401042858022320, 0.2306359803922080343, 5.959266323858941219E-17 ) ) ;
#10992 = ORIENTED_EDGE ( 'NONE', *, *, #23444, .T. ) ;
#10993 = CARTESIAN_POINT ( 'NONE',  ( -26.99999999999959854, -19.33065833018799751, -25.00000000000000000 ) ) ;
#10994 =( BOUNDED_CURVE ( )  B_SPLINE_CURVE ( 2, ( #9058, #11, #14175 ),
 .UNSPECIFIED., .F., .F. ) 
 B_SPLINE_CURVE_WITH_KNOTS ( ( 3, 3 ),
 ( 0.000000000000000000, 0.1752654207116860208 ),
 .UNSPECIFIED. ) 
 CURVE ( )  GEOMETRIC_REPRESENTATION_ITEM ( )  RATIONAL_B_SPLINE_CURVE ( ( 1.000000000000000000, 1.154700538379239916, 1.000000000000000000 ) ) 
 REPRESENTATION_ITEM ( '' )  );
#10995 = ORGANIZATION ( 'NAUO-ORG12', 'UNSPECIFIED', 'UNSPECIFIED' ) ;
#10996 = ITEM_DEFINED_TRANSFORMATION ( 'NONE', 'NONE', #23122,  #18043 ) ;
#10997 = AXIS2_PLACEMENT_3D ( 'NONE', #14291, #15733, #4697 ) ;
#10998 = DIRECTION ( 'NONE',  ( 2.853725266239763049E-28, 3.456932630710235087E-14, 1.000000000000000000 ) ) ;
#10999 = LINE ( 'NONE', #3503, #6192 ) ;
#11000 = CYLINDRICAL_SURFACE ( 'NONE', #2580, 2.500000000000000000 ) ;
#11001 = EDGE_CURVE ( 'NONE', #5106, #9182, #4436, .T. ) ;
#11002 = FACE_OUTER_BOUND ( 'NONE', #13778, .T. ) ;
#11003 = DIRECTION ( 'NONE',  ( -1.138590270679730064E-14, -2.220446049251240387E-15, -1.000000000000000000 ) ) ;
#11004 = CARTESIAN_POINT ( 'NONE',  ( 35.59419854219520118, 9.774809681453278998, -26.50000000000049738 ) ) ;
#11005 = DIRECTION ( 'NONE',  ( 5.034846547286470251E-14, -3.944250458554629736E-32, 1.000000000000000000 ) ) ;
#11006 = DIRECTION ( 'NONE',  ( -1.239096229992449859E-15, -4.969341027244109908E-15, -1.000000000000000000 ) ) ;
#11007 = CIRCLE ( 'NONE', #19717, 2.500000000000000444 ) ;
#11008 = CARTESIAN_POINT ( 'NONE',  ( 2.499999999999970246, -31.09999999999999787, 19.00000000000000000 ) ) ;
#11009 = EDGE_CURVE ( 'NONE', #13082, #14490, #10527, .T. ) ;
#11011 = ORIENTED_EDGE ( 'NONE', *, *, #22775, .F. ) ;
#11010 = EDGE_CURVE ( 'NONE', #12312, #4592, #19997, .T. ) ;
#11012 = VERTEX_POINT ( 'NONE', #14527 ) ;
#11013 = CARTESIAN_POINT ( 'NONE',  ( 35.59419854219520118, 9.774809681453278998, -25.00000000000000000 ) ) ;
#11014 = LINE ( 'NONE', #18370, #4560 ) ;
#11015 = CIRCLE ( 'NONE', #8394, 2.458500000000000352 ) ;
#11016 = EDGE_LOOP ( 'NONE', ( #14059, #3554, #16854, #22026 ) ) ;
#11017 = DIRECTION ( 'NONE',  ( -1.982541115402064913E-15, -6.814985084194598285E-15, 1.000000000000000000 ) ) ;
#11018 = ORIENTED_EDGE ( 'NONE', *, *, #4849, .F. ) ;
#11019 = DIRECTION ( 'NONE',  ( -1.000000000000000000, 2.775557561562891351E-15, 0.000000000000000000 ) ) ;
#11020 = PERSON_AND_ORGANIZATION ( #11966, #8758 ) ;
#11021 = PRODUCT_DEFINITION_SHAPE ( 'NONE', 'NONE',  #23485 ) ;
#11022 = LOCAL_TIME ( 14, 11, 27.00000000000000000, #10712 ) ;
#11023 = SECURITY_CLASSIFICATION_LEVEL ( 'unclassified' ) ;
#11024 = CARTESIAN_POINT ( 'NONE',  ( 120.8143550994449953, 2.935590694028680225, 13.00000000000000000 ) ) ;
#11025 = VECTOR ( 'NONE', #4630, 1000.000000000000114 ) ;
#11026 = EDGE_LOOP ( 'NONE', ( #18333, #16500 ) ) ;
#11027 = EDGE_CURVE ( 'NONE', #9579, #3945, #2928, .T. ) ;
#11028 = DIRECTION ( 'NONE',  ( -6.123237831918409167E-17, 1.616838880122404932E-30, 1.000000000000000000 ) ) ;
#11029 = ORIENTED_EDGE ( 'NONE', *, *, #11985, .T. ) ;
#11030 = CARTESIAN_POINT ( 'NONE',  ( -22.52506283708739687, 28.95208917575130414, -6.749999999995010214 ) ) ;
#11031 = EDGE_CURVE ( 'NONE', #7204, #3206, #11682, .T. ) ;
#11032 = VERTEX_POINT ( 'NONE', #17987 ) ;
#11033 = VECTOR ( 'NONE', #16747, 999.9999999999998863 ) ;
#11034 = CARTESIAN_POINT ( 'NONE',  ( 0.000000000000000000, -17.30000000000000071, -2.500000000000000000 ) ) ;
#11035 = CYLINDRICAL_SURFACE ( 'NONE', #17142, 2.500999999999819590 ) ;
#11036 = DIRECTION ( 'NONE',  ( -2.670035496199930325E-15, -1.152311220646620054E-14, 1.000000000000000000 ) ) ;
#11037 = VERTEX_POINT ( 'NONE', #13454 ) ;
#11038 = ADVANCED_FACE ( 'NONE', ( #7988 ), #2519, .F. ) ;
#11039 = CC_DESIGN_APPROVAL ( #5175, ( #19552 ) ) ;
#11040 = SECURITY_CLASSIFICATION_LEVEL ( 'unclassified' ) ;
#11041 = EDGE_CURVE ( 'NONE', #12652, #255, #2159, .T. ) ;
#11042 = CARTESIAN_POINT ( 'NONE',  ( -65.94066197199057910, 13.04136584699437407, -5.515665073666213751E-15 ) ) ;
#11043 = VERTEX_POINT ( 'NONE', #22109 ) ;
#11044 = PERSON_AND_ORGANIZATION_ROLE ( 'design_supplier' ) ;
#11045 = ORIENTED_EDGE ( 'NONE', *, *, #1508, .F. ) ;
#11046 = ORIENTED_EDGE ( 'NONE', *, *, #11985, .F. ) ;
#11047 = CARTESIAN_POINT ( 'NONE',  ( -69.88753305544580030, 2.884110939634079607, -5.500000000000079048 ) ) ;
#11048 = DATE_AND_TIME ( #7241, #11511 ) ;
#11049 = VECTOR ( 'NONE', #16829, 1000.000000000000227 ) ;
#11050 = FACE_OUTER_BOUND ( 'NONE', #15402, .T. ) ;
#11051 = DATE_AND_TIME ( #14598, #7564 ) ;
#11052 = CARTESIAN_POINT ( 'NONE',  ( -20.00000000000000000, -20.00000000000000000, 5.000000000000000000 ) ) ;
#11053 = APPROVAL_PERSON_ORGANIZATION ( #8782, #10557, #7363 ) ;
#11054 = APPROVAL_PERSON_ORGANIZATION ( #6918, #5465, #14032 ) ;
#11055 = CARTESIAN_POINT ( 'NONE',  ( 118.5079952955230027, -6.794810348829399160, 15.50000000000000000 ) ) ;
#11056 = APPROVAL ( #19627, 'UNSPECIFIED' ) ;
#11057 = CIRCLE ( 'NONE', #20, 2.499999999999998668 ) ;
#11058 = PERSON_AND_ORGANIZATION ( #11966, #8758 ) ;
#11059 = VERTEX_POINT ( 'NONE', #2408 ) ;
#11060 = LOCAL_TIME ( 14, 11, 27.00000000000000000, #19116 ) ;
#11061 = LINE ( 'NONE', #4030, #20377 ) ;
#11062 = VECTOR ( 'NONE', #16662, 1000.000000000000000 ) ;
#11063 = ORIENTED_EDGE ( 'NONE', *, *, #16049, .F. ) ;
#11064 = PERSON ( 'NAUO-PER12', 'UNSPECIFIED', 'UNSPECIFIED', ('UNSPECIFIED'), ('UNSPECIFIED'), ('UNSPECIFIED') ) ;
#11065 = DIRECTION ( 'NONE',  ( -0.2306359803922066187, -0.9730401042858026761, 0.000000000000000000 ) ) ;
#11066 = DIRECTION ( 'NONE',  ( -0.2306359803922080620, -0.9730401042858023430, -1.182825655742500503E-14 ) ) ;
#11067 = FACE_OUTER_BOUND ( 'NONE', #14581, .T. ) ;
#11068 = ORIENTED_EDGE ( 'NONE', *, *, #20723, .F. ) ;
#11069 = VERTEX_POINT ( 'NONE', #15222 ) ;
#11070 = LINE ( 'NONE', #9277, #16303 ) ;
#11071 = VERTEX_POINT ( 'NONE', #9669 ) ;
#11072 = APPROVAL_DATE_TIME ( #23391, #21563 ) ;
#11073 = LOCAL_TIME ( 14, 11, 27.00000000000000000, #8127 ) ;
#11074 = ORIENTED_EDGE ( 'NONE', *, *, #21964, .T. ) ;
#11075 = ORIENTED_EDGE ( 'NONE', *, *, #14177, .F. ) ;
#11076 = DIRECTION ( 'NONE',  ( 0.9730401042858024541, -0.2306359803922080898, -5.959266323858942451E-17 ) ) ;
#11077 = PRODUCT_DEFINITION_FORMATION_WITH_SPECIFIED_SOURCE ( 'ANY', '', #23309, .NOT_KNOWN. ) ;
#11078 = LINE ( 'NONE', #3692, #9945 ) ;
#11079 = PERSON_AND_ORGANIZATION ( #11966, #8758 ) ;
#11080 = VECTOR ( 'NONE', #10687, 1000.000000000000114 ) ;
#11081 = FACE_OUTER_BOUND ( 'NONE', #18137, .T. ) ;
#11082 = EDGE_CURVE ( 'NONE', #2588, #12472, #11690, .T. ) ;
#11083 = DIRECTION ( 'NONE',  ( 0.000000000000000000, 0.000000000000000000, -1.000000000000000000 ) ) ;
#11084 = LOCAL_TIME ( 14, 11, 27.00000000000000000, #3751 ) ;
#11085 = ORIENTED_EDGE ( 'NONE', *, *, #6331, .T. ) ;
#11086 = CARTESIAN_POINT ( 'NONE',  ( -14.54830929662869998, 0.3367883020382160253, -6.749999999996750155 ) ) ;
#11087 = APPROVAL_STATUS ( 'not_yet_approved' ) ;
#11088 = LOCAL_TIME ( 14, 11, 27.00000000000000000, #10852 ) ;
#11089 = ORIENTED_EDGE ( 'NONE', *, *, #14071, .T. ) ;
#11090 = CARTESIAN_POINT ( 'NONE',  ( 35.07420204808331476, 7.580974001528614004, 10.74538000000021043 ) ) ;
#11091 = VECTOR ( 'NONE', #22165, 1000.000000000000000 ) ;
#11092 = CARTESIAN_POINT ( 'NONE',  ( 113.2033677465029911, -29.17473274740290279, -3.099999999999920153 ) ) ;
#11093 = DIRECTION ( 'NONE',  ( 0.005235963827117092427, -0.9999862922474493931, -2.636227439667000721E-16 ) ) ;
#11094 = CARTESIAN_POINT ( 'NONE',  ( -26.00000000000000000, -20.00000000055539928, 5.500000000004630074 ) ) ;
#11095 = CIRCLE ( 'NONE', #75, 2.500000000000001776 ) ;
#11096 = LINE ( 'NONE', #21635, #21682 ) ;
#11097 = VERTEX_POINT ( 'NONE', #22570 ) ;
#11098 = LOCAL_TIME ( 14, 11, 27.00000000000000000, #13861 ) ;
#11099 = DIRECTION ( 'NONE',  ( -7.664170260637049561E-16, -3.491853980616970288E-15, 1.000000000000000000 ) ) ;
#11100 = UNCERTAINTY_MEASURE_WITH_UNIT (LENGTH_MEASURE( 1.000000000000000082E-05 ), #15211, 'distance_accuracy_value', 'NONE');
#11101 = CIRCLE ( 'NONE', #17555, 4.250000000000000000 ) ;
#11102 = VERTEX_POINT ( 'NONE', #4312 ) ;
#11103 = ORIENTED_EDGE ( 'NONE', *, *, #14491, .F. ) ;
#11104 = FACE_OUTER_BOUND ( 'NONE', #11107, .T. ) ;
#11105 = CIRCLE ( 'NONE', #829, 2.750000000000001776 ) ;
#11106 = CARTESIAN_POINT ( 'NONE',  ( 33.97401642954523737, -0.5293161874333298655, -13.00000000000039968 ) ) ;
#11107 = EDGE_LOOP ( 'NONE', ( #9453, #10344, #20545, #2905, #469 ) ) ;
#11108 = FACE_OUTER_BOUND ( 'NONE', #6659, .T. ) ;
#11109 = ADVANCED_FACE ( 'NONE', ( #13101 ), #17121, .F. ) ;
#11110 = VERTEX_POINT ( 'NONE', #2275 ) ;
#11111 = APPROVAL_PERSON_ORGANIZATION ( #11994, #10120, #19453 ) ;
#11112 = FACE_OUTER_BOUND ( 'NONE', #8626, .T. ) ;
#11113 = APPROVAL_STATUS ( 'not_yet_approved' ) ;
#11114 = CONICAL_SURFACE ( 'NONE', #462, 2.283500000000000529, 0.7853981633974469467 ) ;
#11115 = DIRECTION ( 'NONE',  ( -3.210834492181180024E-17, 2.441916418604790135E-15, 1.000000000000000000 ) ) ;
#11116 = AXIS2_PLACEMENT_3D ( 'NONE', #13134, #11369, #533 ) ;
#11117 = CC_DESIGN_PERSON_AND_ORGANIZATION_ASSIGNMENT ( #9961, #2470, ( #18637 ) ) ;
#11118 = AXIS2_PLACEMENT_3D ( 'NONE', #18605, #13715, #20957 ) ;
#11119 = APPLICATION_CONTEXT ( 'configuration controlled 3d designs of mechanical parts and assemblies' ) ;
#11120 = DIRECTION ( 'NONE',  ( -9.096131349985791167E-47, -1.000000000000000000, -2.757014059715200372E-16 ) ) ;
#11121 = EDGE_CURVE ( 'NONE', #9157, #14240, #243, .T. ) ;
#11122 = EDGE_CURVE ( 'NONE', #16084, #7551, #13541, .T. ) ;
#11123 = CIRCLE ( 'NONE', #5399, 4.099999999999999645 ) ;
#11124 = LINE ( 'NONE', #18356, #5221 ) ;
#11125 = DATE_AND_TIME ( #14774, #18995 ) ;
#11126 = CYLINDRICAL_SURFACE ( 'NONE', #5851, 2.500000000000000444 ) ;
#11127 = CIRCLE ( 'NONE', #478, 2.500000000000000444 ) ;
#11128 = DIRECTION ( 'NONE',  ( 0.000000000000000000, 0.000000000000000000, 1.000000000000000000 ) ) ;
#11129 = AXIS2_PLACEMENT_3D ( 'NONE', #12821, #3912, #4026 ) ;
#11130 = CARTESIAN_POINT ( 'NONE',  ( 113.4570673249340018, -28.10438863268850085, 2.700000000000049916 ) ) ;
#11131 = CC_DESIGN_APPROVAL ( #20397, ( #20819 ) ) ;
#11132 = CYLINDRICAL_SURFACE ( 'NONE', #17113, 2.500000000000000000 ) ;
#11133 = LINE ( 'NONE', #21662, #16063 ) ;
#11134 = VECTOR ( 'NONE', #11773, 1000.000000000000114 ) ;
#11135 = DIRECTION ( 'NONE',  ( 0.7071067811865476838, -1.387778780781444689E-15, 0.7071067811865473507 ) ) ;
#11136 = AXIS2_PLACEMENT_3D ( 'NONE', #5731, #16193, #1578 ) ;
#11137 = EDGE_LOOP ( 'NONE', ( #6295, #6002, #4695, #15324 ) ) ;
#11138 = VECTOR ( 'NONE', #21073, 1000.000000000000114 ) ;
#11139 = ORIENTED_EDGE ( 'NONE', *, *, #22385, .F. ) ;
#11140 = CARTESIAN_POINT ( 'NONE',  ( -69.83648240813148789, -6.865755409778319773, -3.000000000000079936 ) ) ;
#11141 = SHAPE_REPRESENTATION ( '1602p_c_06', ( #12739 ), #9323 ) ;
#11142 = CARTESIAN_POINT ( 'NONE',  ( 37.13840842239409312, 23.31972727237319631, -15.00000000000051159 ) ) ;
#11143 = VERTEX_POINT ( 'NONE', #6210 ) ;
#11144 = CARTESIAN_POINT ( 'NONE',  ( -8.080225385240009217, -15.72171916155420313, 2.500000000000000000 ) ) ;
#11145 = EDGE_CURVE ( 'NONE', #14376, #12983, #18688, .T. ) ;
#11146 = VERTEX_POINT ( 'NONE', #4417 ) ;
#11147 = CARTESIAN_POINT ( 'NONE',  ( 37.88245768368250310, -4.127756955731490152, -13.00000000000000000 ) ) ;
#11148 = AXIS2_PLACEMENT_3D ( 'NONE', #5628, #16095, #20117 ) ;
#11149 = MECHANICAL_CONTEXT ( 'NONE', #8221, 'mechanical' ) ;
#11150 = CARTESIAN_POINT ( 'NONE',  ( 35.38043770193282711, 7.701206496806046964, -8.759424124906630027 ) ) ;
#11151 = VECTOR ( 'NONE', #6647, 1000.000000000000227 ) ;
#11152 = APPROVAL ( #9022, 'UNSPECIFIED' ) ;
#11153 = CC_DESIGN_APPROVAL ( #1801, ( #22114 ) ) ;
#11154 = CC_DESIGN_PERSON_AND_ORGANIZATION_ASSIGNMENT ( #6861, #21673, ( #14223 ) ) ;
#11155 = CONTEXT_DEPENDENT_SHAPE_REPRESENTATION ( #9167, #7413 ) ;
#11156 =( NAMED_UNIT ( * ) PLANE_ANGLE_UNIT ( ) SI_UNIT ( $, .RADIAN. ) );
#11157 = CIRCLE ( 'NONE', #13797, 5.999999999999998224 ) ;
#11158 = EDGE_CURVE ( 'NONE', #18339, #18104, #18914, .T. ) ;
#11159 = CIRCLE ( 'NONE', #880, 0.4000000000000001887 ) ;
#11160 = ADVANCED_FACE ( 'NONE', ( #9538 ), #16760, .F. ) ;
#11161 = EDGE_LOOP ( 'NONE', ( #10226, #10571, #17346, #14204 ) ) ;
#11162 = AXIS2_PLACEMENT_3D ( 'NONE', #13689, #20928, #21054 ) ;
#11163 = PRODUCT_RELATED_PRODUCT_CATEGORY ( 'detail', '', ( #19329 ) ) ;
#11164 = CYLINDRICAL_SURFACE ( 'NONE', #5842, 8.250000000000003553 ) ;
#11165 = ORIENTED_EDGE ( 'NONE', *, *, #11185, .F. ) ;
#11166 = CARTESIAN_POINT ( 'NONE',  ( 37.15537257096429613, 9.790160638979559238, 29.25000000000000000 ) ) ;
#11167 = ORIENTED_EDGE ( 'NONE', *, *, #16451, .F. ) ;
#11168 = AXIS2_PLACEMENT_3D ( 'NONE', #5481, #14625, #3690 ) ;
#11169 = CARTESIAN_POINT ( 'NONE',  ( 113.8430260960419957, 8.210644904773758412, 3.037748485030009753E-14 ) ) ;
#11170 = LINE ( 'NONE', #14809, #21312 ) ;
#11171 = LINE ( 'NONE', #18391, #10143 ) ;
#11172 = VERTEX_POINT ( 'NONE', #9892 ) ;
#11173 = AXIS2_PLACEMENT_3D ( 'NONE', #4000, #9112, #3646 ) ;
#11174 = PERSON_AND_ORGANIZATION_ROLE ( 'classification_officer' ) ;
#11175 = LINE ( 'NONE', #9250, #19870 ) ;
#11176 = AXIS2_PLACEMENT_3D ( 'NONE', #21389, #17719, #21150 ) ;
#11177 = EDGE_LOOP ( 'NONE', ( #16121, #4390 ) ) ;
#11178 = PERSON_AND_ORGANIZATION ( #11966, #8758 ) ;
#11179 = CARTESIAN_POINT ( 'NONE',  ( -11.24263882182209962, 20.87636639668270178, -2.500000000000000000 ) ) ;
#11180 = EDGE_CURVE ( 'NONE', #3632, #10657, #15103, .T. ) ;
#11181 = ORIENTED_EDGE ( 'NONE', *, *, #22028, .F. ) ;
#11182 = ORIENTED_EDGE ( 'NONE', *, *, #14612, .T. ) ;
#11183 = DIRECTION ( 'NONE',  ( 6.123230159571619958E-17, 0.000000000000000000, 1.000000000000000000 ) ) ;
#11184 = PERSON_AND_ORGANIZATION ( #11966, #8758 ) ;
#11185 = EDGE_CURVE ( 'NONE', #14730, #3926, #15061, .T. ) ;
#11186 = DIRECTION ( 'NONE',  ( -6.123237831918399306E-17, 1.569224110909209817E-30, 1.000000000000000000 ) ) ;
#11187 = COORDINATED_UNIVERSAL_TIME_OFFSET ( 0, 0, .AHEAD. ) ;
#11188 = CARTESIAN_POINT ( 'NONE',  ( 30.16078946048209630, 0.07586793050039619679, -13.00000000000039968 ) ) ;
#11189 = EDGE_CURVE ( 'NONE', #6737, #15927, #22625, .T. ) ;
#11190 = VECTOR ( 'NONE', #12092, 999.9999999999998863 ) ;
#11191 = ADVANCED_FACE ( 'NONE', ( #13331 ), #11297, .T. ) ;
#11192 = CARTESIAN_POINT ( 'NONE',  ( -26.68810977484059777, -6.639828994528159889, -2.501000000000090484 ) ) ;
#11193 = CONICAL_SURFACE ( 'NONE', #15330, 2.254620000000000513, 0.7853981633974461696 ) ;
#11194 = APPROVAL_STATUS ( 'not_yet_approved' ) ;
#11195 = VERTEX_POINT ( 'NONE', #7625 ) ;
#11196 = DIRECTION ( 'NONE',  ( 0.9999862922464843873, 0.005235964011423952132, 1.932211830181250652E-17 ) ) ;
#11197 = ORIENTED_EDGE ( 'NONE', *, *, #19547, .T. ) ;
#11198 = DIRECTION ( 'NONE',  ( 1.138590270679730064E-14, 2.220446049251240387E-15, 1.000000000000000000 ) ) ;
#11199 = CARTESIAN_POINT ( 'NONE',  ( -20.00000000000000000, -20.00000000000000000, 5.000000000000000000 ) ) ;
#11200 = DIRECTION ( 'NONE',  ( -0.2306359803922028717, -0.9730401042858035643, 4.849856555169150033E-15 ) ) ;
#11201 = ORIENTED_EDGE ( 'NONE', *, *, #22125, .F. ) ;
#11202 = EDGE_LOOP ( 'NONE', ( #6, #13094, #6502, #18965 ) ) ;
#11203 = LINE ( 'NONE', #18894, #6833 ) ;
#11204 = VERTEX_POINT ( 'NONE', #4062 ) ;
#11205 = PERSON_AND_ORGANIZATION ( #11966, #8758 ) ;
#11206 = ORIENTED_EDGE ( 'NONE', *, *, #5037, .T. ) ;
#11207 = ORIENTED_EDGE ( 'NONE', *, *, #8047, .T. ) ;
#11208 = CARTESIAN_POINT ( 'NONE',  ( 30.89467803343009678, -3.022216679643963566, 11.00000000000020606 ) ) ;
#11209 = DIRECTION ( 'NONE',  ( -6.662112528310618598E-09, 1.000000000000000000, -2.081668171172169697E-15 ) ) ;
#11210 = APPROVAL_STATUS ( 'not_yet_approved' ) ;
#11211 = DIRECTION ( 'NONE',  ( 0.9286452767786566032, 1.871119812896368998E-17, -0.3709689338970208472 ) ) ;
#11212 = CARTESIAN_POINT ( 'NONE',  ( -20.00000000397270128, 22.95208919257159863, 5.000000000004460432 ) ) ;
#11213 = EDGE_CURVE ( 'NONE', #4601, #8933, #18566, .T. ) ;
#11214 = VERTEX_POINT ( 'NONE', #14984 ) ;
#11215 = CARTESIAN_POINT ( 'NONE',  ( -65.64475015647069256, -21.84411297095480009, -5.000000000000000000 ) ) ;
#11216 = MECHANICAL_CONTEXT ( 'NONE', #6706, 'mechanical' ) ;
#11217 = CIRCLE ( 'NONE', #10075, 2.999999999999999556 ) ;
#11218 = ORIENTED_EDGE ( 'NONE', *, *, #3881, .T. ) ;
#11219 = FACE_OUTER_BOUND ( 'NONE', #12589, .T. ) ;
#11220 = CARTESIAN_POINT ( 'NONE',  ( 51.98156320189710300, 17.12649442102254937, -13.00000000000000000 ) ) ;
#11221 = CARTESIAN_POINT ( 'NONE',  ( -19.99999999999849720, -20.00000000000000000, 6.500000000004389378 ) ) ;
#11222 = EDGE_CURVE ( 'NONE', #16298, #16051, #15077, .T. ) ;
#11223 = CARTESIAN_POINT ( 'NONE',  ( 52.49909637502329929, -7.592283011512620305, -13.00000000000039968 ) ) ;
#11224 = PLANE ( 'NONE',  #7321 ) ;
#11225 = ORIENTED_EDGE ( 'NONE', *, *, #18006, .T. ) ;
#11226 = CARTESIAN_POINT ( 'NONE',  ( 120.6036919168680015, 2.985523383783529994, -13.00000000000000000 ) ) ;
#11227 = PRODUCT_DEFINITION_SHAPE ( 'NONE', 'NONE',  #23474 ) ;
#11228 = ORIENTED_EDGE ( 'NONE', *, *, #20372, .T. ) ;
#11229 = EDGE_LOOP ( 'NONE', ( #18279, #15788 ) ) ;
#11230 = DIRECTION ( 'NONE',  ( -0.6944962871189153120, 0.7194962871190101472, 0.000000000000000000 ) ) ;
#11231 = CARTESIAN_POINT ( 'NONE',  ( 2.671834669462799905, 17.57827187707419725, -6.695602606842570519E-15 ) ) ;
#11232 = ORIENTED_EDGE ( 'NONE', *, *, #22410, .F. ) ;
#11233 = DIRECTION ( 'NONE',  ( -0.9730401042858036753, 0.2306359803922028995, 5.958148513035547083E-17 ) ) ;
#11234 =( GEOMETRIC_REPRESENTATION_CONTEXT ( 3 ) GLOBAL_UNCERTAINTY_ASSIGNED_CONTEXT ( ( #145 ) ) GLOBAL_UNIT_ASSIGNED_CONTEXT ( ( #895, #21192, #1120 ) ) REPRESENTATION_CONTEXT ( 'NONE', 'WORKASPACE' ) );
#11235 = CARTESIAN_POINT ( 'NONE',  ( 40.45939906362439586, 8.621629779493279244, -2.477422125845284522E-15 ) ) ;
#11236 = CONTEXT_DEPENDENT_SHAPE_REPRESENTATION ( #12765, #11227 ) ;
#11237 = CYLINDRICAL_SURFACE ( 'NONE', #18879, 2.066999999999999726 ) ;
#11238 =( NAMED_UNIT ( * ) SI_UNIT ( $, .STERADIAN. ) SOLID_ANGLE_UNIT ( ) );
#11239 = LINE ( 'NONE', #18466, #14547 ) ;
#11240 = CARTESIAN_POINT ( 'NONE',  ( -20.00000000000000000, -20.00000000000000000, -2.500000000000000000 ) ) ;
#11241 = CALENDAR_DATE ( 2026, 31, 10 ) ;
#11242 = CYLINDRICAL_SURFACE ( 'NONE', #13066, 0.4000000000000001887 ) ;
#11243 = FACE_OUTER_BOUND ( 'NONE', #22420, .T. ) ;
#11244 = EDGE_CURVE ( 'NONE', #9664, #13560, #18497, .T. ) ;
#11245 = LINE ( 'NONE', #18937, #22994 ) ;
#11246 = EDGE_CURVE ( 'NONE', #11330, #14947, #21141, .T. ) ;
#11247 =( GEOMETRIC_REPRESENTATION_CONTEXT ( 3 ) GLOBAL_UNCERTAINTY_ASSIGNED_CONTEXT ( ( #4369 ) ) GLOBAL_UNIT_ASSIGNED_CONTEXT ( ( #17141, #8353, #8007 ) ) REPRESENTATION_CONTEXT ( 'NONE', 'WORKASPACE' ) );
#11248 = DIRECTION ( 'NONE',  ( -0.9286452767786568252, -1.871119812896369614E-17, -0.3709689338970204586 ) ) ;
#11249 = CARTESIAN_POINT ( 'NONE',  ( -20.00000000000000000, -20.00000000000000000, 2.500000000000000000 ) ) ;
#11250 = CARTESIAN_POINT ( 'NONE',  ( -0.5391976746782148888, 18.33937061236850141, 3.301631463538509622E-17 ) ) ;
#11251 = ORIENTED_EDGE ( 'NONE', *, *, #12065, .F. ) ;
#11252 = CIRCLE ( 'NONE', #4024, 5.000000000000000000 ) ;
#11253 = ORIENTED_EDGE ( 'NONE', *, *, #20637, .F. ) ;
#11254 = LINE ( 'NONE', #9450, #11516 ) ;
#11255 = LINE ( 'NONE', #3634, #7595 ) ;
#11256 = VERTEX_POINT ( 'NONE', #8459 ) ;
#11257 = EDGE_CURVE ( 'NONE', #10837, #22163, #15920, .T. ) ;
#11258 = EDGE_CURVE ( 'NONE', #6701, #5973, #7509, .T. ) ;
#11259 = CARTESIAN_POINT ( 'NONE',  ( 36.33124047800322387, 11.14167175084476824, 27.55602540378454535 ) ) ;
#11260 = VERTEX_POINT ( 'NONE', #12146 ) ;
#11261 = FACE_OUTER_BOUND ( 'NONE', #13717, .T. ) ;
#11262 = SHAPE_DEFINITION_REPRESENTATION ( #11624, #6895 ) ;
#11263 = DIRECTION ( 'NONE',  ( -1.000000000000000000, 0.000000000000000000, 0.000000000000000000 ) ) ;
#11264 = CIRCLE ( 'NONE', #3655, 2.499999999999998668 ) ;
#11265 = PERSON_AND_ORGANIZATION_ROLE ( 'classification_officer' ) ;
#11266 = DIRECTION ( 'NONE',  ( 0.0007613694435018767380, -0.9999997101582432935, 0.000000000000000000 ) ) ;
#11267 = VERTEX_POINT ( 'NONE', #11799 ) ;
#11268 = DIRECTION ( 'NONE',  ( -6.123230174520380038E-17, -4.962644601432250805E-15, -1.000000000000000000 ) ) ;
#11269 = EDGE_LOOP ( 'NONE', ( #23036, #10136 ) ) ;
#11270 = LINE ( 'NONE', #13614, #18162 ) ;
#11271 = EDGE_CURVE ( 'NONE', #7533, #21418, #1427, .T. ) ;
#11272 = FACE_BOUND ( 'NONE', #16019, .T. ) ;
#11273 = ORIENTED_EDGE ( 'NONE', *, *, #12351, .T. ) ;
#11274 =( BOUNDED_CURVE ( )  B_SPLINE_CURVE ( 2, ( #2234, #16260, #14079 ),
 .UNSPECIFIED., .F., .F. ) 
 B_SPLINE_CURVE_WITH_KNOTS ( ( 3, 3 ),
 ( 0.1168436138077847686, 0.2336872276155859962 ),
 .UNSPECIFIED. ) 
 CURVE ( )  GEOMETRIC_REPRESENTATION_ITEM ( )  RATIONAL_B_SPLINE_CURVE ( ( 1.077350269189624843, 1.077350269189630394, 1.000000000000000000 ) ) 
 REPRESENTATION_ITEM ( '' )  );
#11275 = DIRECTION ( 'NONE',  ( -2.982858504577314686E-17, 2.441916418604790135E-15, 1.000000000000000000 ) ) ;
#11276 = FACE_OUTER_BOUND ( 'NONE', #14754, .T. ) ;
#11277 = DIRECTION ( 'NONE',  ( -0.9730401042858035643, 0.2306359803922028717, 5.958148513035547083E-17 ) ) ;
#11278 = VERTEX_POINT ( 'NONE', #15700 ) ;
#11279 = APPROVAL ( #19651, 'UNKNOWN' ) ;
#11280 = AXIS2_PLACEMENT_3D ( 'NONE', #10066, #11623, #2913 ) ;
#11281 = CALENDAR_DATE ( 2026, 31, 10 ) ;
#11282 = CC_DESIGN_PERSON_AND_ORGANIZATION_ASSIGNMENT ( #2504, #18668, ( #15459 ) ) ;
#11283 = CIRCLE ( 'NONE', #13146, 2.009240000000000581 ) ;
#11284 = DIRECTION ( 'NONE',  ( -0.9730401042858036753, 0.2306359803922031493, -2.804983810440356829E-16 ) ) ;
#11285 = ORIENTED_EDGE ( 'NONE', *, *, #10881, .T. ) ;
#11286 = EDGE_CURVE ( 'NONE', #12984, #2526, #20913, .T. ) ;
#11287 = EDGE_CURVE ( 'NONE', #18309, #4396, #6755, .T. ) ;
#11288 = PERSON_AND_ORGANIZATION ( #11966, #8758 ) ;
#11289 = CARTESIAN_POINT ( 'NONE',  ( -62.93660361792420588, 12.27413839645710070, 3.322570288448809768E-15 ) ) ;
#11290 = ORIENTED_EDGE ( 'NONE', *, *, #9084, .F. ) ;
#11291 = ORIENTED_EDGE ( 'NONE', *, *, #12930, .F. ) ;
#11292 = EDGE_CURVE ( 'NONE', #14346, #5109, #12271, .T. ) ;
#11293 = LINE ( 'NONE', #18521, #854 ) ;
#11294 = EDGE_CURVE ( 'NONE', #9845, #14376, #1312, .T. ) ;
#11295 = APPROVAL_DATE_TIME ( #18523, #8661 ) ;
#11296 = PERSON_AND_ORGANIZATION ( #23241, #19332 ) ;
#11297 = CONICAL_SURFACE ( 'NONE', #1009, 2.254620000000000513, 0.7853981633974461696 ) ;
#11298 = FACE_OUTER_BOUND ( 'NONE', #12674, .T. ) ;
#11299 = AXIS2_PLACEMENT_3D ( 'NONE', #7536, #382, #2177 ) ;
#11300 = AXIS2_PLACEMENT_3D ( 'NONE', #7256, #3217, #21257 ) ;
#11301 = FACE_OUTER_BOUND ( 'NONE', #20396, .T. ) ;
#11302 = PERSON_AND_ORGANIZATION ( #11966, #8758 ) ;
#11303 = ADVANCED_FACE ( 'NONE', ( #14147 ), #11312, .F. ) ;
#11304 = ORIENTED_EDGE ( 'NONE', *, *, #4613, .T. ) ;
#11305 = CIRCLE ( 'NONE', #6346, 7.599342076785325695 ) ;
#11306 =( REPRESENTATION_RELATIONSHIP ('NONE','NONE', #19303, #9313 ) REPRESENTATION_RELATIONSHIP_WITH_TRANSFORMATION ( #16821 )SHAPE_REPRESENTATION_RELATIONSHIP( ) );
#11307 = DIRECTION ( 'NONE',  ( 3.210834492181180024E-17, -2.441916418604790135E-15, -1.000000000000000000 ) ) ;
#11308 = VERTEX_POINT ( 'NONE', #15809 ) ;
#11309 = CARTESIAN_POINT ( 'NONE',  ( -18.05391955182270181, 22.49081825942809942, -4.900728725074969882E-15 ) ) ;
#11310 = CYLINDRICAL_SURFACE ( 'NONE', #15311, 2.499999999999998668 ) ;
#11311 = FACE_OUTER_BOUND ( 'NONE', #6997, .T. ) ;
#11312 = CONICAL_SURFACE ( 'NONE', #17737, 1.033500000000000529, 1.029744258676650093 ) ;
#11313 = ORIENTED_EDGE ( 'NONE', *, *, #5240, .T. ) ;
#11314 = ORIENTED_EDGE ( 'NONE', *, *, #7006, .T. ) ;
#11315 = DIRECTION ( 'NONE',  ( -3.210834492181045054E-17, 2.441916418604790135E-15, 1.000000000000000000 ) ) ;
#11316 = EDGE_LOOP ( 'NONE', ( #12039, #21323, #1407, #15016 ) ) ;
#11317 = EDGE_CURVE ( 'NONE', #13027, #21933, #2943, .T. ) ;
#11318 = ADVANCED_FACE ( 'NONE', ( #19031 ), #6795, .T. ) ;
#11319 = CALENDAR_DATE ( 2026, 31, 10 ) ;
#11320 = AXIS2_PLACEMENT_3D ( 'NONE', #20386, #9468, #4473 ) ;
#11321 = CIRCLE ( 'NONE', #7133, 5.999999999999999112 ) ;
#11322 = ORIENTED_EDGE ( 'NONE', *, *, #14337, .F. ) ;
#11323 = EDGE_LOOP ( 'NONE', ( #259, #5669, #4129, #11794 ) ) ;
#11324 = DIRECTION ( 'NONE',  ( -0.005235963827108362431, 0.9999862922474493931, 5.936218956694023463E-19 ) ) ;
#11325 = SECURITY_CLASSIFICATION_LEVEL ( 'unclassified' ) ;
#11326 = DIRECTION ( 'NONE',  ( 1.000000000000000000, -1.187319687680469919E-16, 5.345529420184390105E-52 ) ) ;
#11327 = CARTESIAN_POINT ( 'NONE',  ( -65.33043290661754554, 13.65811943861251443, -5.515300856952130332E-15 ) ) ;
#11328 = AXIS2_PLACEMENT_3D ( 'NONE', #23345, #14445, #21800 ) ;
#11329 = AXIS2_PLACEMENT_3D ( 'NONE', #13498, #22383, #765 ) ;
#11330 = VERTEX_POINT ( 'NONE', #17718 ) ;
#11332 = DIRECTION ( 'NONE',  ( 3.099353312215988811E-62, 0.000000000000000000, -1.000000000000000000 ) ) ;
#11331 = AXIS2_PLACEMENT_3D ( 'NONE', #2546, #4207, #18590 ) ;
#11333 = APPLICATION_PROTOCOL_DEFINITION ( 'international standard', 'config_control_design', 1994, #11583 ) ;
#11334 = EDGE_CURVE ( 'NONE', #15518, #14947, #17256, .T. ) ;
#11335 = CIRCLE ( 'NONE', #1820, 12.49999999999999467 ) ;
#11336 = ORIENTED_EDGE ( 'NONE', *, *, #22062, .T. ) ;
#11337 = DIRECTION ( 'NONE',  ( -2.270069654138865127E-15, -1.000000000000000000, -4.543838814073030634E-30 ) ) ;
#11338 = FACE_BOUND ( 'NONE', #18209, .T. ) ;
#11339 = CARTESIAN_POINT ( 'NONE',  ( 61.45890873801150178, 17.00438549795339682, 13.00000000000000000 ) ) ;
#11340 = FACE_OUTER_BOUND ( 'NONE', #10725, .T. ) ;
#11341 = ORIENTED_EDGE ( 'NONE', *, *, #3455, .T. ) ;
#11342 = CARTESIAN_POINT ( 'NONE',  ( 117.1241794131700118, -12.63305097454420078, 15.50000000000000000 ) ) ;
#11343 = EDGE_CURVE ( 'NONE', #21585, #8304, #4842, .T. ) ;
#11344 = COORDINATED_UNIVERSAL_TIME_OFFSET ( 0, 0, .AHEAD. ) ;
#11346 = EDGE_CURVE ( 'NONE', #20851, #20507, #18122, .T. ) ;
#11345 = ORIENTED_EDGE ( 'NONE', *, *, #21173, .F. ) ;
#11347 = VERTEX_POINT ( 'NONE', #2873 ) ;
#11348 = CARTESIAN_POINT ( 'NONE',  ( -16.50000000144900270, -4.350228928667009498, -6.749999999996299849 ) ) ;
#11349 = LINE ( 'NONE', #20580, #3755 ) ;
#11350 = ORIENTED_EDGE ( 'NONE', *, *, #14365, .T. ) ;
#11351 = DATE_TIME_ROLE ( 'classification_date' ) ;
#11352 = DIRECTION ( 'NONE',  ( 0.2306359803922085339, 0.9730401042858022320, 0.000000000000000000 ) ) ;
#11353 = DIRECTION ( 'NONE',  ( -0.9730401042858035643, 0.2306359803922028717, 5.958148513035547083E-17 ) ) ;
#11354 = AXIS2_PLACEMENT_3D ( 'NONE', #5602, #12848, #20083 ) ;
#11355 = CARTESIAN_POINT ( 'NONE',  ( 0.000000000000000000, 0.000000000000000000, -2.500000000000000000 ) ) ;
#11356 = DIRECTION ( 'NONE',  ( -0.9730401042858022320, 0.2306359803922080343, 5.959266323858941219E-17 ) ) ;
#11357 = PERSON_AND_ORGANIZATION ( #11966, #8758 ) ;
#11358 = FACE_BOUND ( 'NONE', #14066, .T. ) ;
#11359 = CARTESIAN_POINT ( 'NONE',  ( 41.24356139695900225, 11.92996613406550033, -18.89999999999999858 ) ) ;
#11360 = CC_DESIGN_PERSON_AND_ORGANIZATION_ASSIGNMENT ( #14893, #7540, ( #1155 ) ) ;
#11361 = CARTESIAN_POINT ( 'NONE',  ( -20.00479999606239900, 1.846597379377900028, -7.999999999995519140 ) ) ;
#11362 = LINE ( 'NONE', #11609, #8781 ) ;
#11363 = CLOSED_SHELL ( 'NONE', ( #14956, #11845, #5496, #17979, #19221, #7596, #22397, #16518, #20698, #14418, #14928, #10816, #8113, #19106, #6769, #15093, #4047, #12854, #23143, #23296, #12686 ) ) ;
#11364 = CARTESIAN_POINT ( 'NONE',  ( -26.00000000397269773, 22.95208919201850151, 5.500000000004529710 ) ) ;
#11365 = CARTESIAN_POINT ( 'NONE',  ( 13.08336378532089839, 15.11046688687759776, -3.694269929671379468E-15 ) ) ;
#11366 = ORIENTED_EDGE ( 'NONE', *, *, #7067, .T. ) ;
#11367 = ADVANCED_BREP_SHAPE_REPRESENTATION ( '', ( #9662, #12739 ), #23107 ) ;
#11368 = ORIENTED_EDGE ( 'NONE', *, *, #19285, .F. ) ;
#11369 = DIRECTION ( 'NONE',  ( 6.123237831918399306E-17, -9.341417679122849747E-31, -1.000000000000000000 ) ) ;
#11370 = LINE ( 'NONE', #4219, #9074 ) ;
#11371 = EDGE_LOOP ( 'NONE', ( #17591, #9174 ) ) ;
#11372 = CARTESIAN_POINT ( 'NONE',  ( 120.8143550994449953, 2.935590694028680225, 13.00000000000000000 ) ) ;
#11373 = VERTEX_POINT ( 'NONE', #10133 ) ;
#11374 = DIRECTION ( 'NONE',  ( -1.000000000000000000, -9.259433497721235207E-11, 1.127570259384904101E-14 ) ) ;
#11375 = DATE_TIME_ROLE ( 'classification_date' ) ;
#11376 = CARTESIAN_POINT ( 'NONE',  ( 36.33263316300890011, 11.71018393288660953, -8.762640023735206896 ) ) ;
#11377 = EDGE_CURVE ( 'NONE', #21873, #8919, #20013, .T. ) ;
#11378 = FACE_OUTER_BOUND ( 'NONE', #21474, .T. ) ;
#11379 = ORIENTED_EDGE ( 'NONE', *, *, #2710, .F. ) ;
#11380 = APPROVAL_PERSON_ORGANIZATION ( #12818, #14864, #20299 ) ;
#11381 = CARTESIAN_POINT ( 'NONE',  ( 32.80472184429622473, 19.68535052198753377, -2.008708621733521550E-15 ) ) ;
#11382 = AXIS2_PLACEMENT_3D ( 'NONE', #9904, #15350, #9549 ) ;
#11383 = ORIENTED_EDGE ( 'NONE', *, *, #21929, .T. ) ;
#11384 = DIRECTION ( 'NONE',  ( 0.000000000000000000, 0.000000000000000000, 1.000000000000000000 ) ) ;
#11385 = EDGE_CURVE ( 'NONE', #6349, #10218, #17365, .T. ) ;
#11386 = CARTESIAN_POINT ( 'NONE',  ( 35.27327876533606599, 27.06496614392705879, 13.00000000000000000 ) ) ;
#11387 = EDGE_LOOP ( 'NONE', ( #16941, #14994, #6684, #21547 ) ) ;
#11388 = DIRECTION ( 'NONE',  ( -0.2306359803922033436, -0.9730401042858034533, 0.000000000000000000 ) ) ;
#11389 = DIRECTION ( 'NONE',  ( 0.9999862922474493931, 0.005235963827108502076, 0.000000000000000000 ) ) ;
#11390 = FACE_OUTER_BOUND ( 'NONE', #7791, .T. ) ;
#11391 = VERTEX_POINT ( 'NONE', #14372 ) ;
#11392 = DIRECTION ( 'NONE',  ( -2.269747459788994803E-13, -2.220446049250320181E-15, -1.000000000000000000 ) ) ;
#11393 = ORIENTED_EDGE ( 'NONE', *, *, #19706, .T. ) ;
#11394 =( REPRESENTATION_RELATIONSHIP ('NONE','NONE', #6895, #2026 ) REPRESENTATION_RELATIONSHIP_WITH_TRANSFORMATION ( #21450 )SHAPE_REPRESENTATION_RELATIONSHIP( ) );
#11395 = APPLICATION_PROTOCOL_DEFINITION ( 'international standard', 'config_control_design', 1994, #8680 ) ;
#11396 = CARTESIAN_POINT ( 'NONE',  ( 30.57814311865390167, -3.583136841839989817, 11.00000000000019895 ) ) ;
#11397 = ORIENTED_EDGE ( 'NONE', *, *, #20598, .T. ) ;
#11398 = ORIENTED_EDGE ( 'NONE', *, *, #7871, .F. ) ;
#11399 = FACE_BOUND ( 'NONE', #7606, .T. ) ;
#11400 = CIRCLE ( 'NONE', #12165, 0.4000000000000001887 ) ;
#11401 = PERSON_AND_ORGANIZATION_ROLE ( 'classification_officer' ) ;
#11402 = AXIS2_PLACEMENT_3D ( 'NONE', #19136, #2733, #13651 ) ;
#11403 = EDGE_CURVE ( 'NONE', #17399, #12644, #22609, .T. ) ;
#11404 = DATE_AND_TIME ( #22536, #2630 ) ;
#11405 = CARTESIAN_POINT ( 'NONE',  ( -56.98461483124570037, -21.79876819407909849, -1.072991366992009803E-14 ) ) ;
#11406 = CIRCLE ( 'NONE', #1132, 6.999999999999997335 ) ;
#11407 = CC_DESIGN_PERSON_AND_ORGANIZATION_ASSIGNMENT ( #17173, #2205, ( #16748 ) ) ;
#11408 =( BOUNDED_CURVE ( )  B_SPLINE_CURVE ( 2, ( #7664, #11142, #16329 ),
 .UNSPECIFIED., .F., .F. ) 
 B_SPLINE_CURVE_WITH_KNOTS ( ( 3, 3 ),
 ( 0.000000000000000000, 0.1168436138077985215 ),
 .UNSPECIFIED. ) 
 CURVE ( )  GEOMETRIC_REPRESENTATION_ITEM ( )  RATIONAL_B_SPLINE_CURVE ( ( 1.000000000000000000, 1.077350269189633725, 1.077350269189629950 ) ) 
 REPRESENTATION_ITEM ( '' )  );
#11409 =( LENGTH_UNIT ( ) NAMED_UNIT ( * ) SI_UNIT ( .MILLI., .METRE. ) );
#11410 = CARTESIAN_POINT ( 'NONE',  ( -20.00000000397090005, 22.95208919256900160, 8.250000000004460432 ) ) ;
#11411 = EDGE_CURVE ( 'NONE', #4396, #19560, #12379, .T. ) ;
#11412 = EDGE_CURVE ( 'NONE', #18262, #8564, #23277, .T. ) ;
#11413 = APPLICATION_PROTOCOL_DEFINITION ( 'international standard', 'config_control_design', 1994, #9897 ) ;
#11414 = PRODUCT_DEFINITION_SHAPE ( 'NONE', 'NONE',  #23479 ) ;
#11415 = APPROVAL_PERSON_ORGANIZATION ( #20878, #22432, #1033 ) ;
#11416 = ORIENTED_EDGE ( 'NONE', *, *, #2113, .F. ) ;
#11417 = AXIS2_PLACEMENT_3D ( 'NONE', #14306, #20008, #21541 ) ;
#11418 = CARTESIAN_POINT ( 'NONE',  ( -27.00000000000000000, -20.00000000000000000, -5.000000000000000000 ) ) ;
#11419 = EDGE_LOOP ( 'NONE', ( #19066, #672, #21596, #22581 ) ) ;
#11420 = AXIS2_PLACEMENT_3D ( 'NONE', #18602, #4457, #2448 ) ;
#11421 = CARTESIAN_POINT ( 'NONE',  ( 58.25686728443110951, 17.76335315678753801, 15.50000000000000000 ) ) ;
#11422 = CARTESIAN_POINT ( 'NONE',  ( 1.406882533891259834, 17.87809865158410005, -7.060250502199809043E-15 ) ) ;
#11423 = CARTESIAN_POINT ( 'NONE',  ( -57.14322836594880073, 8.493908704608589488, 2.318032717970499742E-15 ) ) ;
#11424 = ORIENTED_EDGE ( 'NONE', *, *, #5990, .F. ) ;
#11425 = ORIENTED_EDGE ( 'NONE', *, *, #16093, .T. ) ;
#11426 = CARTESIAN_POINT ( 'NONE',  ( 6.500000000000000000, 0.000000000000000000, -5.000000000000000000 ) ) ;
#11427 = VERTEX_POINT ( 'NONE', #1890 ) ;
#11428 = VECTOR ( 'NONE', #5905, 1000.000000000000000 ) ;
#11429 = APPROVAL_STATUS ( 'not_yet_approved' ) ;
#11430 = ORIENTED_EDGE ( 'NONE', *, *, #19869, .T. ) ;
#11431 = ORIENTED_EDGE ( 'NONE', *, *, #13830, .F. ) ;
#11432 = CARTESIAN_POINT ( 'NONE',  ( 39.37089837072279863, 22.23982225285499936, -13.00000000000049916 ) ) ;
#11433 = CARTESIAN_POINT ( 'NONE',  ( -32.65701080836369385, 9.273987487686079945, -2.500000000000000000 ) ) ;
#11434 = APPROVAL_STATUS ( 'not_yet_approved' ) ;
#11435 = APPLICATION_CONTEXT ( 'configuration controlled 3d designs of mechanical parts and assemblies' ) ;
#11436 = CARTESIAN_POINT ( 'NONE',  ( -22.50000000397430000, 22.95208917591821773, -6.749999999995003108 ) ) ;
#11437 = EDGE_CURVE ( 'NONE', #16515, #9811, #3334, .T. ) ;
#11438 = CC_DESIGN_APPROVAL ( #11882, ( #11807 ) ) ;
#11439 = DIRECTION ( 'NONE',  ( -0.005235963827101452160, 0.9999862922474493931, 5.492442074325202057E-16 ) ) ;
#11440 = CC_DESIGN_SECURITY_CLASSIFICATION ( #7616, ( #11812 ) ) ;
#11441 = CC_DESIGN_DATE_AND_TIME_ASSIGNMENT ( #14704, #9133, ( #10711 ) ) ;
#11442 = CIRCLE ( 'NONE', #10733, 2.499999999999999112 ) ;
#11444 = CC_DESIGN_PERSON_AND_ORGANIZATION_ASSIGNMENT ( #3659, #20044, ( #3293 ) ) ;
#11443 = CC_DESIGN_APPROVAL ( #23109, ( #17878 ) ) ;
#11445 = VECTOR ( 'NONE', #14778, 999.9999999999998863 ) ;
#11446 = EDGE_CURVE ( 'NONE', #23127, #11146, #16975, .T. ) ;
#11447 = ADVANCED_FACE ( 'NONE', ( #9272 ), #8650, .T. ) ;
#11448 = EDGE_LOOP ( 'NONE', ( #14969, #2274, #7263, #20283 ) ) ;
#11449 = LINE ( 'NONE', #5953, #15864 ) ;
#11450 = COORDINATED_UNIVERSAL_TIME_OFFSET ( 0, 0, .AHEAD. ) ;
#11451 = EDGE_LOOP ( 'NONE', ( #3313, #19530, #9236, #20915 ) ) ;
#11452 = CARTESIAN_POINT ( 'NONE',  ( -20.36989857172092044, 17.96579046008427127, -4.999999999995548450 ) ) ;
#11453 = VERTEX_POINT ( 'NONE', #7034 ) ;
#11454 = CC_DESIGN_APPROVAL ( #10430, ( #23156 ) ) ;
#11455 = CARTESIAN_POINT ( 'NONE',  ( 35.59419854219520118, 9.774809681453540122, 26.50000000000000000 ) ) ;
#11456 = CARTESIAN_POINT ( 'NONE',  ( -21.66397194015859640, 11.15562530387989959, -5.000000000000000000 ) ) ;
#11457 = APPROVAL_PERSON_ORGANIZATION ( #2269, #6401, #22327 ) ;
#11458 = ORIENTED_EDGE ( 'NONE', *, *, #18221, .F. ) ;
#11459 = DIRECTION ( 'NONE',  ( -0.8660135325225010172, -0.004534477687579933393, 0.5000000000000001110 ) ) ;
#11460 = CIRCLE ( 'NONE', #17126, 2.499999999999998668 ) ;
#11461 = PERSON_AND_ORGANIZATION_ROLE ( 'creator' ) ;
#11462 = ORIENTED_EDGE ( 'NONE', *, *, #13446, .F. ) ;
#11463 = ORIENTED_EDGE ( 'NONE', *, *, #21947, .F. ) ;
#11464 = LINE ( 'NONE', #374, #19092 ) ;
#11465 = CARTESIAN_POINT ( 'NONE',  ( -62.91249983789201394, 7.670697574599230961, -2.999765877365268008 ) ) ;
#11466 = CC_DESIGN_SECURITY_CLASSIFICATION ( #3831, ( #23489 ) ) ;
#11467 = ORIENTED_EDGE ( 'NONE', *, *, #13068, .F. ) ;
#11468 = DATE_AND_TIME ( #7878, #20912 ) ;
#11469 = CARTESIAN_POINT ( 'NONE',  ( 35.59419854219520118, 9.774809681453518806, 19.56700000000000017 ) ) ;
#11470 = ADVANCED_FACE ( 'NONE', ( #3785 ), #19624, .F. ) ;
#11471 = LINE ( 'NONE', #16538, #22639 ) ;
#11472 = CALENDAR_DATE ( 2026, 31, 10 ) ;
#11473 = DIRECTION ( 'NONE',  ( 1.000000000000000000, -8.255079201972930249E-15, 0.000000000000000000 ) ) ;
#11474 = ADVANCED_FACE ( 'NONE', ( #12829 ), #21732, .T. ) ;
#11475 = SECURITY_CLASSIFICATION ( '', '', #23163 ) ;
#11476 = AXIS2_PLACEMENT_3D ( 'NONE', #17441, #18996, #6520 ) ;
#11477 = FACE_OUTER_BOUND ( 'NONE', #20645, .T. ) ;
#11478 = ADVANCED_FACE ( 'NONE', ( #18060 ), #5123, .F. ) ;
#11479 = DIRECTION ( 'NONE',  ( -0.005235963827121941846, 0.9999862922474492821, 7.400535959148351896E-19 ) ) ;
#11480 = COORDINATED_UNIVERSAL_TIME_OFFSET ( 0, 0, .AHEAD. ) ;
#11481 = EDGE_CURVE ( 'NONE', #16983, #23086, #20757, .T. ) ;
#11482 = CC_DESIGN_APPROVAL ( #18067, ( #13355 ) ) ;
#11483 = DIRECTION ( 'NONE',  ( -0.005235963827108352890, 0.9999862922474493931, 5.936218956694023463E-19 ) ) ;
#11484 = PLANE ( 'NONE',  #9409 ) ;
#11485 = CARTESIAN_POINT ( 'NONE',  ( -26.99999999999960210, -31.09999999999999787, 21.50000000000000000 ) ) ;
#11486 = DIRECTION ( 'NONE',  ( 0.2306359803921919083, 0.9730401042858062288, 1.301042606982611127E-13 ) ) ;
#11487 = CARTESIAN_POINT ( 'NONE',  ( 36.78282996199610722, 11.03463321983590006, 29.25000000000000000 ) ) ;
#11488 = ORIENTED_EDGE ( 'NONE', *, *, #2236, .F. ) ;
#11489 = LOCAL_TIME ( 14, 11, 27.00000000000000000, #4782 ) ;
#11490 = ORIENTED_EDGE ( 'NONE', *, *, #10188, .T. ) ;
#11491 = DIRECTION ( 'NONE',  ( -7.283891156702289181E-32, 2.441916418604790135E-15, 1.000000000000000000 ) ) ;
#11492 = DIRECTION ( 'NONE',  ( -0.9730401042858036753, 0.2306359803922028995, 5.958148513035547083E-17 ) ) ;
#11493 = EDGE_LOOP ( 'NONE', ( #6148, #15979, #18386, #4534 ) ) ;
#11494 = CONICAL_SURFACE ( 'NONE', #5391, 1.033499999999999863, 1.029744258676650093 ) ;
#11495 = AXIS2_PLACEMENT_3D ( 'NONE', #5911, #16702, #7232 ) ;
#11496 = DIRECTION ( 'NONE',  ( -2.982858504577324546E-17, 2.441916418604800390E-15, 1.000000000000000000 ) ) ;
#11497 = ORIENTED_EDGE ( 'NONE', *, *, #3594, .T. ) ;
#11498 = AXIS2_PLACEMENT_3D ( 'NONE', #17429, #20751, #4486 ) ;
#11499 = AXIS2_PLACEMENT_3D ( 'NONE', #7549, #10902, #7203 ) ;
#11500 = CARTESIAN_POINT ( 'NONE',  ( -26.26776695296636888, -28.60000000000000142, -20.76776695296636888 ) ) ;
#11501 = PRODUCT_DEFINITION_SHAPE ( 'NONE', 'NONE',  #3714 ) ;
#11502 = PERSON_AND_ORGANIZATION_ROLE ( 'design_owner' ) ;
#11503 = DIRECTION ( 'NONE',  ( 0.2306359803922032325, 0.9730401042858035643, -1.407521210652540462E-17 ) ) ;
#11504 = CC_DESIGN_PERSON_AND_ORGANIZATION_ASSIGNMENT ( #16875, #4056, ( #12718 ) ) ;
#11505 = AXIS2_PLACEMENT_3D ( 'NONE', #14644, #9065, #19988 ) ;
#11506 = EDGE_CURVE ( 'NONE', #1750, #1608, #5977, .T. ) ;
#11507 = SECURITY_CLASSIFICATION_LEVEL ( 'unclassified' ) ;
#11508 = AXIS2_PLACEMENT_3D ( 'NONE', #18404, #13280, #2114 ) ;
#11509 = DIRECTION ( 'NONE',  ( -0.2306359803922028162, -0.9730401042858034533, 1.407521210652564497E-17 ) ) ;
#11510 = VERTEX_POINT ( 'NONE', #218 ) ;
#11511 = LOCAL_TIME ( 14, 11, 27.00000000000000000, #17033 ) ;
#11512 = DIRECTION ( 'NONE',  ( -1.000000000000000000, 0.000000000000000000, 0.000000000000000000 ) ) ;
#11513 = AXIS2_PLACEMENT_3D ( 'NONE', #21842, #14374, #9038 ) ;
#11514 = EDGE_LOOP ( 'NONE', ( #1187, #11398, #11557, #1929 ) ) ;
#11515 = CARTESIAN_POINT ( 'NONE',  ( 35.59419854219520118, 9.774809681453319854, -20.00000000000000000 ) ) ;
#11516 = VECTOR ( 'NONE', #9218, 999.9999999999998863 ) ;
#11517 = AXIS2_PLACEMENT_3D ( 'NONE', #3834, #19763, #21646 ) ;
#11518 = CYLINDRICAL_SURFACE ( 'NONE', #3807, 2.066999999999997950 ) ;
#11519 = EDGE_LOOP ( 'NONE', ( #10350, #14839 ) ) ;
#11520 = CARTESIAN_POINT ( 'NONE',  ( 27.91817548414393713, -6.133715391986954479, -13.00000000000039968 ) ) ;
#11521 = CARTESIAN_POINT ( 'NONE',  ( -20.00000000000000000, -20.00000000000000000, 5.500000000004559020 ) ) ;
#11522 = ORIENTED_EDGE ( 'NONE', *, *, #15651, .T. ) ;
#11523 = ADVANCED_FACE ( 'NONE', ( #21388 ), #8809, .T. ) ;
#11524 = PERSON_AND_ORGANIZATION_ROLE ( 'classification_officer' ) ;
#11525 = CARTESIAN_POINT ( 'NONE',  ( -20.00000000000000000, -20.00000000000000000, 5.000000000004559908 ) ) ;
#11526 = VECTOR ( 'NONE', #17812, 1000.000000000000000 ) ;
#11527 = VERTEX_POINT ( 'NONE', #19955 ) ;
#11528 = VECTOR ( 'NONE', #13287, 1000.000000000000227 ) ;
#11529 = CALENDAR_DATE ( 2026, 31, 10 ) ;
#11530 = DIRECTION ( 'NONE',  ( -0.9730401042858035643, 0.2306359803922028717, 5.958148513035547083E-17 ) ) ;
#11531 = CC_DESIGN_SECURITY_CLASSIFICATION ( #2395, ( #14124 ) ) ;
#11532 = VERTEX_POINT ( 'NONE', #21603 ) ;
#11533 = ORIENTED_EDGE ( 'NONE', *, *, #17800, .T. ) ;
#11534 = CARTESIAN_POINT ( 'NONE',  ( -20.00000000000180123, -20.00000000000000000, -7.999999999995469402 ) ) ;
#11535 = APPROVAL_STATUS ( 'not_yet_approved' ) ;
#11536 = CIRCLE ( 'NONE', #16802, 2.750000000000002220 ) ;
#11537 = CIRCLE ( 'NONE', #1253, 2.499999999999998668 ) ;
#11538 = AXIS2_PLACEMENT_3D ( 'NONE', #13928, #12392, #3348 ) ;
#11539 = DATE_TIME_ROLE ( 'classification_date' ) ;
#11540 = CARTESIAN_POINT ( 'NONE',  ( -20.00000000000000000, -20.00000000000000000, -5.000000000000000000 ) ) ;
#11542 = AXIS2_PLACEMENT_3D ( 'NONE', #3376, #1590, #7424 ) ;
#11541 = FACE_OUTER_BOUND ( 'NONE', #20533, .T. ) ;
#11543 = ORIENTED_EDGE ( 'NONE', *, *, #13905, .T. ) ;
#11544 = DATE_AND_TIME ( #6281, #5682 ) ;
#11545 = LOCAL_TIME ( 14, 11, 27.00000000000000000, #1936 ) ;
#11546 = CIRCLE ( 'NONE', #12666, 2.499999999999999112 ) ;
#11547 = ORIENTED_EDGE ( 'NONE', *, *, #15007, .T. ) ;
#11548 = VECTOR ( 'NONE', #19722, 1000.000000000000000 ) ;
#11549 = CYLINDRICAL_SURFACE ( 'NONE', #798, 5.000000000000000888 ) ;
#11550 = ORIENTED_EDGE ( 'NONE', *, *, #2135, .T. ) ;
#11551 = EDGE_CURVE ( 'NONE', #6032, #5808, #5233, .T. ) ;
#11552 = DIRECTION ( 'NONE',  ( 0.9730401042858035643, -0.2306359803922028717, -5.958148513035547083E-17 ) ) ;
#11553 = AXIS2_PLACEMENT_3D ( 'NONE', #4598, #11866, #670 ) ;
#11554 = DIRECTION ( 'NONE',  ( 0.7071067811865475727, 0.000000000000000000, -0.7071067811865474617 ) ) ;
#11555 = CARTESIAN_POINT ( 'NONE',  ( -20.00000000397270128, 22.95208919257349933, 5.500000000004459544 ) ) ;
#11556 = ORIENTED_EDGE ( 'NONE', *, *, #16305, .F. ) ;
#11557 = ORIENTED_EDGE ( 'NONE', *, *, #323, .T. ) ;
#11558 = DIRECTION ( 'NONE',  ( -1.000000000000000000, 2.275047181608927151E-16, 0.000000000000000000 ) ) ;
#11559 = ORIENTED_EDGE ( 'NONE', *, *, #21964, .F. ) ;
#11560 = APPLICATION_PROTOCOL_DEFINITION ( 'international standard', 'config_control_design', 1994, #15179 ) ;
#11561 = ORIENTED_EDGE ( 'NONE', *, *, #18037, .T. ) ;
#11562 = ORIENTED_EDGE ( 'NONE', *, *, #9076, .F. ) ;
#11563 = CARTESIAN_POINT ( 'NONE',  ( 120.2377651484647032, 0.5029904333151411500, -13.00000000000000000 ) ) ;
#11564 = DATE_AND_TIME ( #16867, #5388 ) ;
#11565 = EDGE_CURVE ( 'NONE', #3018, #4601, #3316, .T. ) ;
#11566 = CARTESIAN_POINT ( 'NONE',  ( -22.99999999999959854, -19.33065833018789803, -25.00000000000000000 ) ) ;
#11567 = EDGE_CURVE ( 'NONE', #187, #8431, #10721, .T. ) ;
#11568 = CONICAL_SURFACE ( 'NONE', #22899, 2.729132938682640397, 1.047197551196598297 ) ;
#11569 = CYLINDRICAL_SURFACE ( 'NONE', #16536, 4.750000000000001776 ) ;
#11570 = AXIS2_PLACEMENT_3D ( 'NONE', #21949, #12943, #14836 ) ;
#11571 = DIRECTION ( 'NONE',  ( 0.000000000000000000, 0.000000000000000000, 1.000000000000000000 ) ) ;
#11572 = DIRECTION ( 'NONE',  ( -0.9997648975362222190, -0.02168293463503410262, 0.000000000000000000 ) ) ;
#11573 = COORDINATED_UNIVERSAL_TIME_OFFSET ( 0, 0, .AHEAD. ) ;
#11574 = EDGE_LOOP ( 'NONE', ( #18273, #19993, #19764, #20504 ) ) ;
#11575 = DIRECTION ( 'NONE',  ( -0.9730401042858035643, 0.2306359803922028717, 5.958148513035547083E-17 ) ) ;
#11576 = CARTESIAN_POINT ( 'NONE',  ( 61.55522920193588021, -1.517168634553750062, 1.006920016453334892E-14 ) ) ;
#11577 = ORIENTED_EDGE ( 'NONE', *, *, #10031, .T. ) ;
#11578 = EDGE_CURVE ( 'NONE', #9430, #687, #9021, .T. ) ;
#11579 = DIRECTION ( 'NONE',  ( -0.9997648975362221080, -0.02168293463503390486, 0.000000000000000000 ) ) ;
#11580 = FACE_OUTER_BOUND ( 'NONE', #820, .T. ) ;
#11581 = ORIENTED_EDGE ( 'NONE', *, *, #18059, .F. ) ;
#11582 = CARTESIAN_POINT ( 'NONE',  ( 28.14554285793940025, -3.006546890859489896, 11.00000000000019895 ) ) ;
#11583 = APPLICATION_CONTEXT ( 'configuration controlled 3d designs of mechanical parts and assemblies' ) ;
#11584 = CC_DESIGN_PERSON_AND_ORGANIZATION_ASSIGNMENT ( #13955, #9942, ( #9377 ) ) ;
#11585 = APPROVAL_ROLE ( '' ) ;
#11586 = ORIENTED_EDGE ( 'NONE', *, *, #19414, .F. ) ;
#11587 = APPROVAL ( #8887, 'UNSPECIFIED' ) ;
#11588 = ORIENTED_EDGE ( 'NONE', *, *, #2863, .T. ) ;
#11589 = DIRECTION ( 'NONE',  ( -1.296622928517387947E-46, 1.000000000000000000, -1.557192143389729909E-30 ) ) ;
#11590 = DIRECTION ( 'NONE',  ( -0.9997651245102160411, -0.02167246670483410909, 0.000000000000000000 ) ) ;
#11591 = ORIENTED_EDGE ( 'NONE', *, *, #10118, .F. ) ;
#11592 = PERSON_AND_ORGANIZATION ( #11966, #8758 ) ;
#11593 = ADVANCED_FACE ( 'NONE', ( #5346 ), #22074, .T. ) ;
#11594 = LINE ( 'NONE', #18702, #14148 ) ;
#11595 = EDGE_CURVE ( 'NONE', #13995, #14120, #9385, .T. ) ;
#11596 = CC_DESIGN_DATE_AND_TIME_ASSIGNMENT ( #7589, #3916, ( #1978 ) ) ;
#11597 = DIRECTION ( 'NONE',  ( -0.2867834340965179085, 0.9579954394086686031, -4.640009386119478376E-15 ) ) ;
#11598 = APPROVAL_ROLE ( '' ) ;
#11599 = EDGE_CURVE ( 'NONE', #1063, #3048, #4079, .T. ) ;
#11600 = DIRECTION ( 'NONE',  ( -0.8823529412199823119, 0.4705882352125332901, 8.962737959213505425E-15 ) ) ;
#11601 = CARTESIAN_POINT ( 'NONE',  ( 32.79777292954499757, -5.491820719290810615, 13.00000000000019895 ) ) ;
#11602 = CIRCLE ( 'NONE', #1317, 3.499999999999999556 ) ;
#11603 = PLANE ( 'NONE',  #21908 ) ;
#11604 = MECHANICAL_CONTEXT ( 'NONE', #17631, 'mechanical' ) ;
#11605 = DIRECTION ( 'NONE',  ( -0.9730401042858035643, 0.2306359803922031215, -2.740969466505752002E-16 ) ) ;
#11606 = LINE ( 'NONE', #16660, #18524 ) ;
#11607 = PLANE ( 'NONE',  #2116 ) ;
#11608 = EDGE_CURVE ( 'NONE', #9579, #22503, #14960, .T. ) ;
#11609 = CARTESIAN_POINT ( 'NONE',  ( 39.83668191656649782, 5.994421497922050257, 19.59999999999999787 ) ) ;
#11610 = DIRECTION ( 'NONE',  ( 0.2306359803922080620, 0.9730401042858023430, -4.744007713284279563E-15 ) ) ;
#11611 = ORIENTED_EDGE ( 'NONE', *, *, #16961, .T. ) ;
#11612 = AXIS2_PLACEMENT_3D ( 'NONE', #6756, #1149, #6509 ) ;
#11613 = ORIENTED_EDGE ( 'NONE', *, *, #13415, .T. ) ;
#11614 = DIRECTION ( 'NONE',  ( 0.005235963827108232327, -0.9999862922474493931, -5.936218956694023463E-19 ) ) ;
#11615 = LINE ( 'NONE', #22505, #4515 ) ;
#11616 = ORIENTED_EDGE ( 'NONE', *, *, #413, .F. ) ;
#11617 = EDGE_CURVE ( 'NONE', #11726, #6764, #22269, .T. ) ;
#11618 = LINE ( 'NONE', #8150, #14523 ) ;
#11619 = EDGE_LOOP ( 'NONE', ( #21072, #21524 ) ) ;
#11620 = EDGE_CURVE ( 'NONE', #9018, #16515, #18537, .T. ) ;
#11621 = LINE ( 'NONE', #15378, #1122 ) ;
#11622 = PERSON_AND_ORGANIZATION ( #11966, #8758 ) ;
#11623 = DIRECTION ( 'NONE',  ( -2.269747459788994803E-13, -2.220446049250320181E-15, -1.000000000000000000 ) ) ;
#11624 = PRODUCT_DEFINITION_SHAPE ( 'NONE', 'NONE',  #10854 ) ;
#11625 = DIRECTION ( 'NONE',  ( -3.210834492181054915E-17, 2.441916418604790135E-15, 1.000000000000000000 ) ) ;
#11626 = DIRECTION ( 'NONE',  ( -1.187319687680494078E-16, -2.805478249478340539E-20, -1.000000000000000000 ) ) ;
#11627 = CARTESIAN_POINT ( 'NONE',  ( 29.27674327513866004, 1.765923432495702716, 13.00000000000019895 ) ) ;
#11628 = ORIENTED_EDGE ( 'NONE', *, *, #17355, .T. ) ;
#11629 = DIRECTION ( 'NONE',  ( -1.000000000000000000, 0.000000000000000000, 0.000000000000000000 ) ) ;
#11630 = AXIS2_PLACEMENT_3D ( 'NONE', #9322, #7197, #23328 ) ;
#11631 = EDGE_CURVE ( 'NONE', #11097, #6893, #16607, .T. ) ;
#11632 = DIRECTION ( 'NONE',  ( 0.000000000000000000, 1.734723475976806848E-16, 1.000000000000000000 ) ) ;
#11633 = ORIENTED_EDGE ( 'NONE', *, *, #6081, .F. ) ;
#11634 = CARTESIAN_POINT ( 'NONE',  ( 39.83668191656649782, 5.994421497922050257, 19.59999999999999787 ) ) ;
#11635 = DIRECTION ( 'NONE',  ( -0.7071067811865475727, 1.387778780781445281E-15, 0.7071067811865475727 ) ) ;
#11636 = ORIENTED_EDGE ( 'NONE', *, *, #15055, .F. ) ;
#11637 = COORDINATED_UNIVERSAL_TIME_OFFSET ( 0, 0, .AHEAD. ) ;
#11638 = FACE_OUTER_BOUND ( 'NONE', #14911, .T. ) ;
#11639 = EDGE_CURVE ( 'NONE', #5508, #19958, #9808, .T. ) ;
#11640 = VERTEX_POINT ( 'NONE', #9503 ) ;
#11641 = EDGE_CURVE ( 'NONE', #1750, #8186, #6047, .T. ) ;
#11642 = CALENDAR_DATE ( 2026, 31, 10 ) ;
#11643 = CARTESIAN_POINT ( 'NONE',  ( -20.00000000397270128, 22.95208919256889857, -5.448922613368719782E-15 ) ) ;
#11644 = ORIENTED_EDGE ( 'NONE', *, *, #21381, .F. ) ;
#11645 = EDGE_LOOP ( 'NONE', ( #5862, #9541, #20655, #9934 ) ) ;
#11646 = PERSON_AND_ORGANIZATION_ROLE ( 'design_owner' ) ;
#11647 = VECTOR ( 'NONE', #21481, 1000.000000000000114 ) ;
#11648 = APPROVAL_ROLE ( '' ) ;
#11649 = DIRECTION ( 'NONE',  ( -0.9999862922474492821, -0.005235963827122071951, 1.466966272681990292E-16 ) ) ;
#11650 = DIRECTION ( 'NONE',  ( 9.412241839989958199E-48, -1.000000000000000000, 2.441916418604790135E-15 ) ) ;
#11651 = ORIENTED_EDGE ( 'NONE', *, *, #9104, .T. ) ;
#11652 = APPROVAL_STATUS ( 'not_yet_approved' ) ;
#11653 = AXIS2_PLACEMENT_3D ( 'NONE', #594, #5840, #11326 ) ;
#11654 = VECTOR ( 'NONE', #5877, 1000.000000000000000 ) ;
#11655 = EDGE_LOOP ( 'NONE', ( #8095, #16113, #17093, #18484, #14263 ) ) ;
#11656 = DIRECTION ( 'NONE',  ( -0.9730401042858035643, 0.2306359803922028717, 5.432877459303547053E-17 ) ) ;
#11657 = DIRECTION ( 'NONE',  ( 0.9730401042858036753, -0.2306359803922031493, 2.804983810440361760E-16 ) ) ;
#11658 = ORIENTED_EDGE ( 'NONE', *, *, #22062, .F. ) ;
#11659 = CYLINDRICAL_SURFACE ( 'NONE', #10579, 0.0009999999999615351298 ) ;
#11660 = CARTESIAN_POINT ( 'NONE',  ( 117.8160873543469904, -9.713930661686799084, 3.415130773183659557E-14 ) ) ;
#11661 = CARTESIAN_POINT ( 'NONE',  ( 2.499999999999970246, -28.60000000000000142, 19.00000000000000000 ) ) ;
#11662 = VERTEX_POINT ( 'NONE', #11421 ) ;
#11663 = ORIENTED_EDGE ( 'NONE', *, *, #2694, .F. ) ;
#11664 = DIRECTION ( 'NONE',  ( -1.000000000000000000, 0.000000000000000000, 0.000000000000000000 ) ) ;
#11665 = ORIENTED_EDGE ( 'NONE', *, *, #17872, .F. ) ;
#11666 = COORDINATED_UNIVERSAL_TIME_OFFSET ( 0, 0, .AHEAD. ) ;
#11667 = ADVANCED_BREP_SHAPE_REPRESENTATION ( '', ( #17588, #12739 ), #20713 ) ;
#11668 = VERTEX_POINT ( 'NONE', #331 ) ;
#11669 = ORIENTED_EDGE ( 'NONE', *, *, #19242, .F. ) ;
#11670 = DIRECTION ( 'NONE',  ( -0.9730401042858035643, 0.2306359803922028717, 5.958148513035547083E-17 ) ) ;
#11671 = SECURITY_CLASSIFICATION_LEVEL ( 'unclassified' ) ;
#11672 = DIRECTION ( 'NONE',  ( -1.000000000000000000, 0.000000000000000000, 0.000000000000000000 ) ) ;
#11673 = VECTOR ( 'NONE', #12433, 1000.000000000000000 ) ;
#11674 = CONICAL_SURFACE ( 'NONE', #10912, 2.283499999999998753, 0.7853981633974433940 ) ;
#11675 = VECTOR ( 'NONE', #1689, 1000.000000000000000 ) ;
#11676 = ADVANCED_FACE ( 'NONE', ( #5826 ), #11659, .F. ) ;
#11677 = DIRECTION ( 'NONE',  ( 1.000000000000000000, 0.000000000000000000, 0.000000000000000000 ) ) ;
#11678 = AXIS2_PLACEMENT_3D ( 'NONE', #9554, #20348, #2292 ) ;
#11679 = DIRECTION ( 'NONE',  ( 6.123237831918409167E-17, -1.613784273878194890E-30, -1.000000000000000000 ) ) ;
#11680 = APPLICATION_PROTOCOL_DEFINITION ( 'international standard', 'config_control_design', 1994, #15946 ) ;
#11681 = VERTEX_POINT ( 'NONE', #456 ) ;
#11682 = CIRCLE ( 'NONE', #5956, 4.999999999999996447 ) ;
#11683 = CARTESIAN_POINT ( 'NONE',  ( -58.47878404538157326, -8.306306658711820390, -5.528360538656855117E-15 ) ) ;
#11684 = CARTESIAN_POINT ( 'NONE',  ( -60.05196788195259927, 12.68574396146170180, -5.000000000000000000 ) ) ;
#11685 = EDGE_LOOP ( 'NONE', ( #16519, #11379 ) ) ;
#11686 = ADVANCED_FACE ( 'NONE', ( #4149 ), #3923, .F. ) ;
#11687 = ADVANCED_FACE ( 'NONE', ( #7597 ), #5617, .T. ) ;
#11688 = AXIS2_PLACEMENT_3D ( 'NONE', #22922, #11679, #13547 ) ;
#11689 = AXIS2_PLACEMENT_3D ( 'NONE', #15267, #18954, #13722 ) ;
#11690 = LINE ( 'NONE', #18450, #1410 ) ;
#11691 = AXIS2_PLACEMENT_3D ( 'NONE', #21601, #12487, #14143 ) ;
#11692 = CYLINDRICAL_SURFACE ( 'NONE', #7682, 2.499999999999998668 ) ;
#11693 = ORIENTED_EDGE ( 'NONE', *, *, #13472, .T. ) ;
#11694 = DIRECTION ( 'NONE',  ( 6.124378941434239724E-17, -2.274246353359159970E-33, 1.000000000000000000 ) ) ;
#11695 = APPROVAL_STATUS ( 'not_yet_approved' ) ;
#11696 = EDGE_LOOP ( 'NONE', ( #936, #20529, #10811, #18133 ) ) ;
#11697 = ORIENTED_EDGE ( 'NONE', *, *, #22186, .T. ) ;
#11698 = DIRECTION ( 'NONE',  ( -0.9730401042858024541, 0.2306359803922080898, 5.959266323858942451E-17 ) ) ;
#11699 = CARTESIAN_POINT ( 'NONE',  ( -26.00000000000000000, -20.00000000055539928, 6.750000000004630074 ) ) ;
#11700 = ORIENTED_EDGE ( 'NONE', *, *, #11317, .T. ) ;
#11701 = APPROVAL_DATE_TIME ( #4431, #17941 ) ;
#11702 = DIRECTION ( 'NONE',  ( 0.9999862922474491711, 0.005235963827116866913, -1.514467536079854800E-31 ) ) ;
#11703 = DIRECTION ( 'NONE',  ( -0.2306359803922080620, -0.9730401042858023430, 6.358253941197272741E-15 ) ) ;
#11704 = DATE_TIME_ROLE ( 'classification_date' ) ;
#11705 = DIRECTION ( 'NONE',  ( 1.466984912809907930E-16, 2.805478249466195144E-20, 1.000000000000000000 ) ) ;
#11706 = CIRCLE ( 'NONE', #23037, 2.500000000000000444 ) ;
#11707 = EDGE_CURVE ( 'NONE', #11832, #15489, #18888, .T. ) ;
#11708 = CIRCLE ( 'NONE', #15475, 3.499999999999999556 ) ;
#11709 = CC_DESIGN_PERSON_AND_ORGANIZATION_ASSIGNMENT ( #2777, #4677, ( #22886 ) ) ;
#11710 = CARTESIAN_POINT ( 'NONE',  ( 39.27359436029389883, 22.26288585089424998, -13.00000000000030020 ) ) ;
#11711 = PERSON_AND_ORGANIZATION ( #11966, #8758 ) ;
#11712 = CC_DESIGN_PERSON_AND_ORGANIZATION_ASSIGNMENT ( #17104, #593, ( #576 ) ) ;
#11713 = DIRECTION ( 'NONE',  ( -0.9730401042858036753, 0.2306359803922023999, -1.110223024625155524E-17 ) ) ;
#11714 = CARTESIAN_POINT ( 'NONE',  ( -57.14322836594880073, 8.493908704608589488, 2.318032717970499742E-15 ) ) ;
#11715 = ADVANCED_FACE ( 'NONE', ( #13077, #9862, #693 ), #7958, .T. ) ;
#11716 = EDGE_CURVE ( 'NONE', #3009, #2498, #4391, .T. ) ;
#11717 = DIRECTION ( 'NONE',  ( 2.269747459788994803E-13, 2.220446049250605354E-15, 1.000000000000000000 ) ) ;
#11718 = PLANE ( 'NONE',  #7257 ) ;
#11719 = VECTOR ( 'NONE', #655, 999.9999999999998863 ) ;
#11720 = FACE_OUTER_BOUND ( 'NONE', #9646, .T. ) ;
#11721 = ORIENTED_EDGE ( 'NONE', *, *, #9493, .T. ) ;
#11722 = ORIENTED_EDGE ( 'NONE', *, *, #17238, .F. ) ;
#11723 = DIRECTION ( 'NONE',  ( -0.8660135325225002401, -0.004534477687579664511, -0.5000000000000014433 ) ) ;
#11724 = CIRCLE ( 'NONE', #15491, 3.499999999999999556 ) ;
#11725 = DIRECTION ( 'NONE',  ( 0.000000000000000000, 0.000000000000000000, -1.000000000000000000 ) ) ;
#11726 = VERTEX_POINT ( 'NONE', #14835 ) ;
#11727 = DIRECTION ( 'NONE',  ( -3.099353312215989243E-62, 1.403547063447849893E-77, 1.000000000000000000 ) ) ;
#11728 = EDGE_LOOP ( 'NONE', ( #6085, #17545, #6892, #7859 ) ) ;
#11729 = FACE_OUTER_BOUND ( 'NONE', #16885, .T. ) ;
#11730 = APPROVAL_ROLE ( '' ) ;
#11731 = CARTESIAN_POINT ( 'NONE',  ( -17.50000000000180123, -19.99999998334472195, -7.999999999996036060 ) ) ;
#11732 = EDGE_CURVE ( 'NONE', #8200, #8090, #20194, .T. ) ;
#11733 = ITEM_DEFINED_TRANSFORMATION ( 'NONE', 'NONE', #13126,  #12739 ) ;
#11734 = DIRECTION ( 'NONE',  ( -0.2306359803922038432, -0.9730401042858032312, 5.139921410301653163E-15 ) ) ;
#11735 = CC_DESIGN_PERSON_AND_ORGANIZATION_ASSIGNMENT ( #12253, #8318, ( #6911 ) ) ;
#11736 = CC_DESIGN_DATE_AND_TIME_ASSIGNMENT ( #19962, #3686, ( #6084 ) ) ;
#11737 = AXIS2_PLACEMENT_3D ( 'NONE', #11924, #8450, #19252 ) ;
#11738 = DIRECTION ( 'NONE',  ( 0.000000000000000000, -1.000000000000000000, 0.000000000000000000 ) ) ;
#11739 = VERTEX_POINT ( 'NONE', #18422 ) ;
#11740 = DIRECTION ( 'NONE',  ( -3.210834492181040124E-17, 2.441916418604790135E-15, 1.000000000000000000 ) ) ;
#11741 = ADVANCED_FACE ( 'NONE', ( #8190 ), #19130, .F. ) ;
#11742 = EDGE_CURVE ( 'NONE', #551, #1544, #1290, .T. ) ;
#11743 = CARTESIAN_POINT ( 'NONE',  ( -66.29618031796869104, -0.3471291603817620031, 3.000000000000100364 ) ) ;
#11744 = EDGE_LOOP ( 'NONE', ( #5241, #13168, #3576, #16844 ) ) ;
#11745 = DIRECTION ( 'NONE',  ( -9.248855984704951398E-11, 1.000000000000000000, -2.220446048198180498E-15 ) ) ;
#11746 = DIRECTION ( 'NONE',  ( -2.982858504577314686E-17, 2.441916418604790135E-15, 1.000000000000000000 ) ) ;
#11747 = COORDINATED_UNIVERSAL_TIME_OFFSET ( 0, 0, .AHEAD. ) ;
#11748 = CARTESIAN_POINT ( 'NONE',  ( -20.00000000397270128, 22.95208919257159863, 5.000000000004460432 ) ) ;
#11749 = VERTEX_POINT ( 'NONE', #10341 ) ;
#11750 = PERSON_AND_ORGANIZATION_ROLE ( 'design_supplier' ) ;
#11751 = LINE ( 'NONE', #13750, #14866 ) ;
#11752 = VERTEX_POINT ( 'NONE', #4741 ) ;
#11753 = ORIENTED_EDGE ( 'NONE', *, *, #20530, .F. ) ;
#11754 = SHAPE_DEFINITION_REPRESENTATION ( #20690, #15060 ) ;
#11755 = EDGE_CURVE ( 'NONE', #12528, #1775, #2847, .T. ) ;
#11756 = DATE_AND_TIME ( #14951, #12206 ) ;
#11757 =( BOUNDED_CURVE ( )  B_SPLINE_CURVE ( 2, ( #16085, #23316, #11965 ),
 .UNSPECIFIED., .F., .F. ) 
 B_SPLINE_CURVE_WITH_KNOTS ( ( 3, 3 ),
 ( 0.000000000000000000, 0.1168436138077930952 ),
 .UNSPECIFIED. ) 
 CURVE ( )  GEOMETRIC_REPRESENTATION_ITEM ( )  RATIONAL_B_SPLINE_CURVE ( ( 1.000000000000000000, 1.077350269189630172, 1.077350269189629950 ) ) 
 REPRESENTATION_ITEM ( '' )  );
#11758 = CARTESIAN_POINT ( 'NONE',  ( 30.72899802076640086, 10.92798958341530025, -1.881607274541729715E-15 ) ) ;
#11759 = SECURITY_CLASSIFICATION ( '', '', #17137 ) ;
#11760 = AXIS2_PLACEMENT_3D ( 'NONE', #2058, #257, #8960 ) ;
#11761 = EDGE_CURVE ( 'NONE', #4807, #17568, #14716, .T. ) ;
#11762 = DIRECTION ( 'NONE',  ( -1.000000000000000000, 0.000000000000000000, 0.000000000000000000 ) ) ;
#11763 = VERTEX_POINT ( 'NONE', #2955 ) ;
#11764 = ADVANCED_FACE ( 'NONE', ( #1041 ), #2728, .T. ) ;
#11765 = APPROVAL_STATUS ( 'not_yet_approved' ) ;
#11766 = EDGE_CURVE ( 'NONE', #4039, #12528, #7895, .T. ) ;
#11767 = VERTEX_POINT ( 'NONE', #20887 ) ;
#11768 = CARTESIAN_POINT ( 'NONE',  ( 34.89491389100820129, 23.30074776265919922, 13.00000000000000000 ) ) ;
#11769 = DIRECTION ( 'NONE',  ( -0.2306359803922054252, -0.9730401042858028982, 0.000000000000000000 ) ) ;
#11770 = ORIENTED_EDGE ( 'NONE', *, *, #400, .F. ) ;
#11771 = CARTESIAN_POINT ( 'NONE',  ( 119.9163041628193440, 1.024182177979823027, -13.00000000000000000 ) ) ;
#11772 = CARTESIAN_POINT ( 'NONE',  ( 43.84419854219520118, 9.774809681453278998, 21.49999999999999289 ) ) ;
#11773 = DIRECTION ( 'NONE',  ( -0.7070970883417647679, -0.003702385528188428636, -0.7071067811865467956 ) ) ;
#11774 = CIRCLE ( 'NONE', #14779, 6.500000000000000888 ) ;
#11775 = ORIENTED_EDGE ( 'NONE', *, *, #17042, .T. ) ;
#11776 = ORIENTED_EDGE ( 'NONE', *, *, #17400, .T. ) ;
#11778 = LINE ( 'NONE', #8311, #21970 ) ;
#11777 = CIRCLE ( 'NONE', #11402, 6.499999999999997335 ) ;
#11779 = ORIENTED_EDGE ( 'NONE', *, *, #2599, .T. ) ;
#11780 = DATE_AND_TIME ( #6183, #4957 ) ;
#11781 = ORIENTED_EDGE ( 'NONE', *, *, #16143, .T. ) ;
#11782 = EDGE_LOOP ( 'NONE', ( #1342, #6354, #22927, #14968 ) ) ;
#11783 = CYLINDRICAL_SURFACE ( 'NONE', #11894, 3.499999999999999112 ) ;
#11784 = CIRCLE ( 'NONE', #2653, 4.399999999999997691 ) ;
#11785 = DATE_TIME_ROLE ( 'classification_date' ) ;
#11786 = CARTESIAN_POINT ( 'NONE',  ( 40.42677426225490933, 27.12808637232325282, -13.00000000000030020 ) ) ;
#11787 = CC_DESIGN_PERSON_AND_ORGANIZATION_ASSIGNMENT ( #11793, #13799, ( #4225 ) ) ;
#11788 = LOCAL_TIME ( 14, 11, 27.00000000000000000, #9378 ) ;
#11789 =( NAMED_UNIT ( * ) PLANE_ANGLE_UNIT ( ) SI_UNIT ( $, .RADIAN. ) );
#11790 =( GEOMETRIC_REPRESENTATION_CONTEXT ( 3 ) GLOBAL_UNCERTAINTY_ASSIGNED_CONTEXT ( ( #8955 ) ) GLOBAL_UNIT_ASSIGNED_CONTEXT ( ( #5114, #6671, #4876 ) ) REPRESENTATION_CONTEXT ( 'NONE', 'WORKASPACE' ) );
#11791 = AXIS2_PLACEMENT_3D ( 'NONE', #9097, #18132, #17695 ) ;
#11792 = CARTESIAN_POINT ( 'NONE',  ( -65.82123935389580538, 11.86253283145240012, -5.000000000000000000 ) ) ;
#11793 = PERSON_AND_ORGANIZATION ( #11966, #8758 ) ;
#11794 = ORIENTED_EDGE ( 'NONE', *, *, #21893, .F. ) ;
#11795 = CARTESIAN_POINT ( 'NONE',  ( 2.500000000000000000, -30.47499999999999787, -19.00000000000000000 ) ) ;
#11796 = CARTESIAN_POINT ( 'NONE',  ( 39.87324790931398866, 24.79279012203729948, -13.00000000000049916 ) ) ;
#11797 = AXIS2_PLACEMENT_3D ( 'NONE', #21036, #19257, #23034 ) ;
#11798 = ORIENTED_EDGE ( 'NONE', *, *, #12888, .F. ) ;
#11799 = CARTESIAN_POINT ( 'NONE',  ( 34.43023877205762062, 1.829043660892390566, -13.00000000000000000 ) ) ;
#11800 = DIRECTION ( 'NONE',  ( -0.9730401042858024541, 0.2306359803922080898, 5.959266323858942451E-17 ) ) ;
#11801 = AXIS2_PLACEMENT_3D ( 'NONE', #8592, #10856, #3234 ) ;
#11802 = ORIENTED_EDGE ( 'NONE', *, *, #1863, .F. ) ;
#11803 = LINE ( 'NONE', #13677, #13379 ) ;
#11804 = DATE_AND_TIME ( #4532, #17083 ) ;
#11805 = ADVANCED_FACE ( 'NONE', ( #15671 ), #22545, .T. ) ;
#11806 = PRODUCT ( 'Base Frame Plate', 'Base Frame Plate', '', ( #2087 ) ) ;
#11807 = SECURITY_CLASSIFICATION ( '', '', #10255 ) ;
#11808 = ORIENTED_EDGE ( 'NONE', *, *, #16491, .T. ) ;
#11809 = ORIENTED_EDGE ( 'NONE', *, *, #22429, .T. ) ;
#11810 = CARTESIAN_POINT ( 'NONE',  ( -21.99996573044222004, -0.1151926037937907599, -1.072055041842232962E-14 ) ) ;
#11811 = DIRECTION ( 'NONE',  ( -0.7194962871189606313, -0.6944962871189667153, 0.000000000000000000 ) ) ;
#11812 = PRODUCT_DEFINITION_FORMATION_WITH_SPECIFIED_SOURCE ( 'ANY', '', #19526, .NOT_KNOWN. ) ;
#11813 = EDGE_LOOP ( 'NONE', ( #16697, #1032 ) ) ;
#11814 = APPLICATION_PROTOCOL_DEFINITION ( 'international standard', 'config_control_design', 1994, #22918 ) ;
#11815 = DIRECTION ( 'NONE',  ( -1.115264941341835834E-15, 3.837966487416229483E-32, -1.000000000000000000 ) ) ;
#11816 = CARTESIAN_POINT ( 'NONE',  ( 35.59419854219520118, 9.774809681453319854, -19.56700000000000017 ) ) ;
#11817 = COORDINATED_UNIVERSAL_TIME_OFFSET ( 0, 0, .AHEAD. ) ;
#11818 = CARTESIAN_POINT ( 'NONE',  ( 5.026060663935580067E-16, -1.434026569662460006E-15, 2.500000000000090150 ) ) ;
#11819 = AXIS2_PLACEMENT_3D ( 'NONE', #17053, #663, #20736 ) ;
#11820 = SHAPE_REPRESENTATION_RELATIONSHIP ( 'NONE' , 'NONE' ,  #12037, #11667 ) ;
#11821 = FACE_OUTER_BOUND ( 'NONE', #7937, .T. ) ;
#11822 = PERSON_AND_ORGANIZATION_ROLE ( 'creator' ) ;
#11823 = CC_DESIGN_APPROVAL ( #6483, ( #3293 ) ) ;
#11824 = APPROVAL_PERSON_ORGANIZATION ( #240, #2186, #14978 ) ;
#11825 = DIRECTION ( 'NONE',  ( -0.9730401042858024541, 0.2306359803922080898, 5.959266323858942451E-17 ) ) ;
#11826 = CARTESIAN_POINT ( 'NONE',  ( 35.93893384793820189, -10.44995626450799975, 3.100000000000000089 ) ) ;
#11827 = DIRECTION ( 'NONE',  ( -0.9730401042858024541, 0.2306359803922080898, 5.959266323858942451E-17 ) ) ;
#11828 = DIRECTION ( 'NONE',  ( 0.9730401042858036753, -0.2306359803922028995, 2.740969466505749537E-16 ) ) ;
#11829 = CARTESIAN_POINT ( 'NONE',  ( 118.4388045014059969, -7.086722380115159758, -19.59999999999999787 ) ) ;
#11830 = CC_DESIGN_APPROVAL ( #1502, ( #3831 ) ) ;
#11831 = CARTESIAN_POINT ( 'NONE',  ( -21.99941281109913760, -0.1562838609880432272, 5.000000000000000000 ) ) ;
#11832 = VERTEX_POINT ( 'NONE', #15783 ) ;
#11833 = EDGE_CURVE ( 'NONE', #23388, #17339, #4855, .T. ) ;
#11834 = ORIENTED_EDGE ( 'NONE', *, *, #9701, .T. ) ;
#11835 = DIRECTION ( 'NONE',  ( 0.9730401042858035643, -0.2306359803922028717, -5.959266323858667582E-17 ) ) ;
#11836 = CARTESIAN_POINT ( 'NONE',  ( 30.89467803343009678, -3.022216679644093240, -15.00000000000039968 ) ) ;
#11837 = VERTEX_POINT ( 'NONE', #18999 ) ;
#11838 = APPROVAL ( #16358, 'UNKNOWN' ) ;
#11839 = DIRECTION ( 'NONE',  ( 0.7071067811865475727, 0.000000000000000000, -0.7071067811865474617 ) ) ;
#11840 = VERTEX_POINT ( 'NONE', #12119 ) ;
#11841 = LOCAL_TIME ( 14, 11, 27.00000000000000000, #2424 ) ;
#11842 = CARTESIAN_POINT ( 'NONE',  ( 29.89447396975359794, -1.047702001783019865, -11.00000000000039968 ) ) ;
#11843 = COORDINATED_UNIVERSAL_TIME_OFFSET ( 0, 0, .AHEAD. ) ;
#11844 = DIRECTION ( 'NONE',  ( 0.2306359803922094498, 0.9730401042858018990, 0.000000000000000000 ) ) ;
#11845 = ADVANCED_FACE ( 'NONE', ( #8305 ), #15540, .T. ) ;
#11846 = ADVANCED_FACE ( 'NONE', ( #20771 ), #17444, .T. ) ;
#11847 = VECTOR ( 'NONE', #5134, 999.9999999999998863 ) ;
#11848 = DATE_TIME_ROLE ( 'classification_date' ) ;
#11849 = APPROVAL_STATUS ( 'not_yet_approved' ) ;
#11850 =( REPRESENTATION_RELATIONSHIP ('NONE','NONE', #6895, #5348 ) REPRESENTATION_RELATIONSHIP_WITH_TRANSFORMATION ( #17546 )SHAPE_REPRESENTATION_RELATIONSHIP( ) );
#11851 = CARTESIAN_POINT ( 'NONE',  ( -1.041857140317360209, 16.21867887107149997, 4.500000000000000000 ) ) ;
#11852 = CARTESIAN_POINT ( 'NONE',  ( 39.37089837072289811, 22.23982225285510239, 15.50000000000000000 ) ) ;
#11853 = CARTESIAN_POINT ( 'NONE',  ( 53.20239347634441884, 27.69690417850089759, 2.500000000000052847 ) ) ;
#11854 = ORIENTED_EDGE ( 'NONE', *, *, #23193, .T. ) ;
#11855 = CARTESIAN_POINT ( 'NONE',  ( -20.00000000000149925, -20.00000000000000000, -6.749999999995469402 ) ) ;
#11856 = PRODUCT_DEFINITION_FORMATION_WITH_SPECIFIED_SOURCE ( 'ANY', '', #2832, .NOT_KNOWN. ) ;
#11857 = CARTESIAN_POINT ( 'NONE',  ( 43.98050001724080005, -5.573152644851309567, 10.50000000000019895 ) ) ;
#11858 = VERTEX_POINT ( 'NONE', #15315 ) ;
#11859 = CYLINDRICAL_SURFACE ( 'NONE', #17724, 2.500999999999819590 ) ;
#11860 = VECTOR ( 'NONE', #10982, 1000.000000000000000 ) ;
#11861 = DIRECTION ( 'NONE',  ( -8.911056267098788616E-18, -1.998401444326210262E-15, -1.000000000000000000 ) ) ;
#11862 = EDGE_CURVE ( 'NONE', #7334, #1184, #17765, .T. ) ;
#11863 = CALENDAR_DATE ( 2026, 31, 10 ) ;
#11864 = VECTOR ( 'NONE', #8888, 1000.000000000000227 ) ;
#11865 = CIRCLE ( 'NONE', #15585, 5.999999999999998224 ) ;
#11866 = DIRECTION ( 'NONE',  ( -0.9730401042858035643, 0.2306359803922028717, -2.804983810440358308E-16 ) ) ;
#11867 = ORIENTED_EDGE ( 'NONE', *, *, #7083, .F. ) ;
#11868 = LOCAL_TIME ( 14, 11, 27.00000000000000000, #10080 ) ;
#11869 = VERTEX_POINT ( 'NONE', #4501 ) ;
#11871 = PERSON_AND_ORGANIZATION ( #11966, #8758 ) ;
#11870 = CC_DESIGN_PERSON_AND_ORGANIZATION_ASSIGNMENT ( #1352, #996, ( #17948 ) ) ;
#11872 = CONICAL_SURFACE ( 'NONE', #12982, 2.283500000000000085, 0.7853981633974469467 ) ;
#11873 = CARTESIAN_POINT ( 'NONE',  ( 37.46113131852679601, -4.027891576221660053, -13.00000000000000000 ) ) ;
#11874 = VERTEX_POINT ( 'NONE', #11771 ) ;
#11875 = APPROVAL ( #9129, 'UNSPECIFIED' ) ;
#11876 = AXIS2_PLACEMENT_3D ( 'NONE', #18071, #2035, #23290 ) ;
#11877 = DIRECTION ( 'NONE',  ( -0.9730401042858035643, 0.2306359803922028717, 5.958148513035547083E-17 ) ) ;
#11878 = APPROVAL_STATUS ( 'not_yet_approved' ) ;
#11879 = EDGE_CURVE ( 'NONE', #4039, #9763, #9996, .T. ) ;
#11880 = EDGE_CURVE ( 'NONE', #16162, #10008, #2685, .T. ) ;
#11881 = LOCAL_TIME ( 14, 11, 27.00000000000000000, #1411 ) ;
#11882 = APPROVAL ( #22934, 'UNSPECIFIED' ) ;
#11883 = SECURITY_CLASSIFICATION_LEVEL ( 'unclassified' ) ;
#11884 = DIRECTION ( 'NONE',  ( 1.000000000000000000, -2.269747459789000104E-13, -7.174648137343060814E-44 ) ) ;
#11885 = VECTOR ( 'NONE', #21605, 1000.000000000000227 ) ;
#11886 = CIRCLE ( 'NONE', #16787, 12.50000000000000000 ) ;
#11887 = AXIS2_PLACEMENT_3D ( 'NONE', #13138, #58, #16228 ) ;
#11888 = CARTESIAN_POINT ( 'NONE',  ( -59.87132660632070014, -21.81388311970430038, 5.000000000000000000 ) ) ;
#11889 = ORIENTED_EDGE ( 'NONE', *, *, #21739, .F. ) ;
#11890 = APPLICATION_CONTEXT ( 'configuration controlled 3d designs of mechanical parts and assemblies' ) ;
#11891 = AXIS2_PLACEMENT_3D ( 'NONE', #1338, #8607, #3248 ) ;
#11892 = APPROVAL_DATE_TIME ( #9748, #22432 ) ;
#11893 = ORIENTED_EDGE ( 'NONE', *, *, #18710, .F. ) ;
#11894 = AXIS2_PLACEMENT_3D ( 'NONE', #21130, #17347, #1053 ) ;
#11895 = CYLINDRICAL_SURFACE ( 'NONE', #7648, 7.000000000000000888 ) ;
#11896 = LINE ( 'NONE', #12005, #16171 ) ;
#11897 = ORIENTED_EDGE ( 'NONE', *, *, #15334, .F. ) ;
#11898 = ADVANCED_FACE ( 'NONE', ( #417 ), #9407, .F. ) ;
#11899 = LOCAL_TIME ( 14, 11, 27.00000000000000000, #8999 ) ;
#11900 = DIRECTION ( 'NONE',  ( 1.138590270679730064E-14, 2.220446049251240387E-15, 1.000000000000000000 ) ) ;
#11901 = CARTESIAN_POINT ( 'NONE',  ( -29.94686441333699989, 7.343408934390579290, 2.500000000000000000 ) ) ;
#11902 = ORIENTED_EDGE ( 'NONE', *, *, #13697, .F. ) ;
#11903 = VERTEX_POINT ( 'NONE', #20274 ) ;
#11904 = PLANE ( 'NONE',  #744 ) ;
#11905 = CIRCLE ( 'NONE', #17951, 3.499999999999999556 ) ;
#11906 = ORIENTED_EDGE ( 'NONE', *, *, #5924, .F. ) ;
#11907 = AXIS2_PLACEMENT_3D ( 'NONE', #7634, #7759, #18698 ) ;
#11908 = COORDINATED_UNIVERSAL_TIME_OFFSET ( 0, 0, .AHEAD. ) ;
#11909 = EDGE_CURVE ( 'NONE', #687, #11308, #2208, .T. ) ;
#11910 = ORIENTED_EDGE ( 'NONE', *, *, #4288, .F. ) ;
#11911 = VECTOR ( 'NONE', #6329, 1000.000000000000000 ) ;
#11912 = ORIENTED_EDGE ( 'NONE', *, *, #11411, .T. ) ;
#11913 = FACE_OUTER_BOUND ( 'NONE', #6491, .T. ) ;
#11914 = SHAPE_REPRESENTATION ( '1602p_c_25', ( #12739 ), #22737 ) ;
#11915 = APPROVAL_DATE_TIME ( #23130, #12161 ) ;
#11916 = EDGE_CURVE ( 'NONE', #9474, #22213, #10191, .T. ) ;
#11917 = ADVANCED_FACE ( 'NONE', ( #11378 ), #3997, .T. ) ;
#11918 = DIRECTION ( 'NONE',  ( -0.9730401042858024541, 0.2306359803922080898, 5.959266323858942451E-17 ) ) ;
#11919 = CONICAL_SURFACE ( 'NONE', #20600, 0.8660254037844397068, 1.047197551196598297 ) ;
#11920 = CC_DESIGN_SECURITY_CLASSIFICATION ( #22114, ( #6956 ) ) ;
#11921 = AXIS2_PLACEMENT_3D ( 'NONE', #15387, #22620, #11512 ) ;
#11922 = VECTOR ( 'NONE', #3628, 1000.000000000000000 ) ;
#11923 = PERSON ( 'NAUO-PER35', 'UNSPECIFIED', 'UNSPECIFIED', ('UNSPECIFIED'), ('UNSPECIFIED'), ('UNSPECIFIED') ) ;
#11924 = CARTESIAN_POINT ( 'NONE',  ( 115.8700071457750056, -9.252658700902388844, 3.427049305831379237E-14 ) ) ;
#11925 = PERSON_AND_ORGANIZATION ( #11966, #8758 ) ;
#11926 = AXIS2_PLACEMENT_3D ( 'NONE', #19670, #11987, #10663 ) ;
#11927 = EDGE_LOOP ( 'NONE', ( #48, #18297, #10817, #564, #16772, #3099 ) ) ;
#11928 = CARTESIAN_POINT ( 'NONE',  ( 33.27836309399499015, 10.32372331478700644, 26.87999999999999901 ) ) ;
#11929 = FACE_OUTER_BOUND ( 'NONE', #17687, .T. ) ;
#11930 = EDGE_LOOP ( 'NONE', ( #8673, #10879, #4500, #10229 ) ) ;
#11931 = DIRECTION ( 'NONE',  ( -0.2306359803922033713, -0.9730401042858033422, 1.407521210652564805E-17 ) ) ;
#11932 = DIRECTION ( 'NONE',  ( -2.982858504577324546E-17, 2.441916418604790135E-15, 1.000000000000000000 ) ) ;
#11933 = FACE_OUTER_BOUND ( 'NONE', #22268, .T. ) ;
#11934 = EDGE_LOOP ( 'NONE', ( #15975, #242, #2799, #18790 ) ) ;
#11935 = CARTESIAN_POINT ( 'NONE',  ( 28.74475271207850113, -0.4785145432219160000, -11.50000000000039968 ) ) ;
#11936 = COORDINATED_UNIVERSAL_TIME_OFFSET ( 0, 0, .AHEAD. ) ;
#11937 = CIRCLE ( 'NONE', #10048, 2.500000000000000444 ) ;
#11938 = ORIENTED_EDGE ( 'NONE', *, *, #2999, .F. ) ;
#11939 = VERTEX_POINT ( 'NONE', #6011 ) ;
#11940 = FACE_OUTER_BOUND ( 'NONE', #5964, .T. ) ;
#11941 = DIRECTION ( 'NONE',  ( -3.469446951953605354E-14, -1.084202172485501657E-13, 1.000000000000000000 ) ) ;
#11942 = EDGE_CURVE ( 'NONE', #16977, #5808, #15032, .T. ) ;
#11943 = EDGE_LOOP ( 'NONE', ( #6746, #11291, #7077, #14092 ) ) ;
#11944 = AXIS2_PLACEMENT_3D ( 'NONE', #11199, #20310, #22193 ) ;
#11945 = PERSON_AND_ORGANIZATION_ROLE ( 'creator' ) ;
#11946 = DIRECTION ( 'NONE',  ( -0.9730401042858024541, 0.2306359803922080898, 5.959266323858942451E-17 ) ) ;
#11947 = DIRECTION ( 'NONE',  ( -0.2306359803922085339, -0.9730401042858022320, 0.000000000000000000 ) ) ;
#11948 = DATE_TIME_ROLE ( 'classification_date' ) ;
#11949 = CYLINDRICAL_SURFACE ( 'NONE', #12080, 3.499999999999999556 ) ;
#11950 = ADVANCED_FACE ( 'NONE', ( #17177 ), #13574, .F. ) ;
#11951 = FACE_OUTER_BOUND ( 'NONE', #10334, .T. ) ;
#11952 = CALENDAR_DATE ( 2026, 31, 10 ) ;
#11953 = CIRCLE ( 'NONE', #15273, 3.499999999999998668 ) ;
#11954 = CARTESIAN_POINT ( 'NONE',  ( 0.03403376487640590031, -6.499910899608420500, -8.889944397045749129E-14 ) ) ;
#11955 = PLANE ( 'NONE',  #5568 ) ;
#11956 = CARTESIAN_POINT ( 'NONE',  ( 58.73439644601039333, 17.65016624305030035, 13.00000000000000000 ) ) ;
#11957 = CARTESIAN_POINT ( 'NONE',  ( -20.00000000397420052, 22.95208919256889857, 8.750000000004618528 ) ) ;
#11958 = DIRECTION ( 'NONE',  ( 0.005235963827102643048, -0.9999862922474495042, 7.723249237701186312E-15 ) ) ;
#11959 = EDGE_LOOP ( 'NONE', ( #18947, #8660, #19266, #16479 ) ) ;
#11960 = PRODUCT ( 'Latching', 'Latching', '', ( #5323 ) ) ;
#11961 = ORIENTED_EDGE ( 'NONE', *, *, #21093, .T. ) ;
#11962 = CARTESIAN_POINT ( 'NONE',  ( 34.24686308852899685, 12.59635270528730011, -2.500000000000000000 ) ) ;
#11963 = FACE_OUTER_BOUND ( 'NONE', #17420, .T. ) ;
#11964 = ORIENTED_EDGE ( 'NONE', *, *, #21995, .F. ) ;
#11965 = CARTESIAN_POINT ( 'NONE',  ( 31.01827548281339020, -2.500766059351007708, 11.00000000000020428 ) ) ;
#11966 = PERSON ( 'UNSPECIFIED', 'UNSPECIFIED', 'UNSPECIFIED', ('UNSPECIFIED'), ('UNSPECIFIED'), ('UNSPECIFIED') ) ;
#11967 = ORIENTED_EDGE ( 'NONE', *, *, #14009, .T. ) ;
#11968 = CARTESIAN_POINT ( 'NONE',  ( 55.46237324781409939, -8.294657213477510282, 13.00000000000000000 ) ) ;
#11969 = CALENDAR_DATE ( 2026, 31, 10 ) ;
#11970 = DIRECTION ( 'NONE',  ( 0.000000000000000000, 1.020425574104004122E-16, 1.000000000000000000 ) ) ;
#11971 = PERSON_AND_ORGANIZATION ( #13039, #19423 ) ;
#11972 = EDGE_CURVE ( 'NONE', #19822, #16162, #16993, .T. ) ;
#11973 = CARTESIAN_POINT ( 'NONE',  ( 36.88454136754629076, -6.460491836936111731, -13.00000000000000000 ) ) ;
#11974 = EDGE_CURVE ( 'NONE', #10214, #8174, #3329, .T. ) ;
#11975 = DIRECTION ( 'NONE',  ( -0.9730401042858035643, 0.2306359803922028717, 5.958148513035547083E-17 ) ) ;
#11976 = DIRECTION ( 'NONE',  ( 0.000000000000000000, 0.000000000000000000, 1.000000000000000000 ) ) ;
#11977 = DIRECTION ( 'NONE',  ( -1.000000000000000000, 2.270069654138870255E-15, 0.000000000000000000 ) ) ;
#11978 = ORIENTED_EDGE ( 'NONE', *, *, #9231, .T. ) ;
#11979 = PLANE ( 'NONE',  #1028 ) ;
#11980 = AXIS2_PLACEMENT_3D ( 'NONE', #15904, #10392, #19829 ) ;
#11981 = DIRECTION ( 'NONE',  ( -3.210834492181045054E-17, 2.441916418604790135E-15, 1.000000000000000000 ) ) ;
#11982 = ORIENTED_EDGE ( 'NONE', *, *, #4870, .F. ) ;
#11983 = DIRECTION ( 'NONE',  ( 1.213490492418610097E-15, 4.861311874477940294E-15, 1.000000000000000000 ) ) ;
#11984 = DIRECTION ( 'NONE',  ( 0.9999862922474492821, 0.005235963827122071951, -1.466966272681990292E-16 ) ) ;
#11985 = EDGE_CURVE ( 'NONE', #5109, #16036, #13964, .T. ) ;
#11986 = EDGE_CURVE ( 'NONE', #2485, #2335, #6368, .T. ) ;
#11987 = DIRECTION ( 'NONE',  ( 0.9730401042858035643, -0.2306359803922028717, 2.804983810440357815E-16 ) ) ;
#11988 = EDGE_LOOP ( 'NONE', ( #13974, #6422, #8785, #21582 ) ) ;
#11989 = ORIENTED_EDGE ( 'NONE', *, *, #19575, .F. ) ;
#11990 = MECHANICAL_CONTEXT ( 'NONE', #19592, 'mechanical' ) ;
#11991 = FACE_OUTER_BOUND ( 'NONE', #19812, .T. ) ;
#11992 = ORIENTED_EDGE ( 'NONE', *, *, #16524, .T. ) ;
#11993 = DIRECTION ( 'NONE',  ( -0.2306359803922032603, -0.9730401042858034533, 0.000000000000000000 ) ) ;
#11994 = PERSON_AND_ORGANIZATION ( #11966, #8758 ) ;
#11995 = AXIS2_PLACEMENT_3D ( 'NONE', #14453, #21679, #19921 ) ;
#11996 = DATE_AND_TIME ( #21218, #17510 ) ;
#11997 = CARTESIAN_POINT ( 'NONE',  ( 34.14207834813670672, 22.29249582057180135, -15.00000000000049916 ) ) ;
#11998 = ADVANCED_FACE ( 'NONE', ( #7678 ), #16823, .T. ) ;
#11999 = DIRECTION ( 'NONE',  ( -0.005235963827101446089, 0.9999862922474493931, 7.400535959109775519E-19 ) ) ;
#12000 = ORIENTED_EDGE ( 'NONE', *, *, #20211, .T. ) ;
#12001 = APPROVAL ( #11113, 'UNKNOWN' ) ;
#12002 = PRODUCT_RELATED_PRODUCT_CATEGORY ( 'detail', '', ( #14223 ) ) ;
#12003 = VERTEX_POINT ( 'NONE', #4359 ) ;
#12004 = DIRECTION ( 'NONE',  ( -3.099353312215988811E-62, 0.000000000000000000, 1.000000000000000000 ) ) ;
#12005 = CARTESIAN_POINT ( 'NONE',  ( 112.2904587062726876, 7.080247408215292637, -13.00000000000000000 ) ) ;
#12006 = VERTEX_POINT ( 'NONE', #18749 ) ;
#12007 = EDGE_CURVE ( 'NONE', #935, #7324, #20731, .T. ) ;
#12008 = EDGE_CURVE ( 'NONE', #21187, #15073, #6773, .T. ) ;
#12009 = CARTESIAN_POINT ( 'NONE',  ( 35.59419854219520118, 9.774809681453550780, 27.87500000000000000 ) ) ;
#12010 = DIRECTION ( 'NONE',  ( -2.972463603623604872E-47, -1.000000000000000000, -2.972463603623604872E-47 ) ) ;
#12011 = CARTESIAN_POINT ( 'NONE',  ( -17.50000000000130029, -19.99999998334472195, -5.499999999996036948 ) ) ;
#12012 = ORIENTED_EDGE ( 'NONE', *, *, #17143, .T. ) ;
#12013 = ORIENTED_EDGE ( 'NONE', *, *, #236, .T. ) ;
#12014 = DIRECTION ( 'NONE',  ( -1.239096229992449859E-15, -4.969341027244109908E-15, -1.000000000000000000 ) ) ;
#12015 = ORIENTED_EDGE ( 'NONE', *, *, #17909, .T. ) ;
#12016 = SHAPE_DEFINITION_REPRESENTATION ( #1306, #20817 ) ;
#12017 = CIRCLE ( 'NONE', #4400, 2.750000000000002220 ) ;
#12018 = ORIENTED_EDGE ( 'NONE', *, *, #22734, .F. ) ;
#12019 = ORIENTED_EDGE ( 'NONE', *, *, #4125, .T. ) ;
#12020 = PLANE ( 'NONE',  #16774 ) ;
#12021 = SHAPE_DEFINITION_REPRESENTATION ( #16888, #7169 ) ;
#12022 = DIRECTION ( 'NONE',  ( -9.594916218540590128E-33, 2.583840697242805182E-16, -1.000000000000000000 ) ) ;
#12023 = ADVANCED_FACE ( 'NONE', ( #13147 ), #20381, .F. ) ;
#12024 = AXIS2_PLACEMENT_3D ( 'NONE', #7503, #12627, #17970 ) ;
#12025 = CIRCLE ( 'NONE', #14284, 3.000000000000000444 ) ;
#12026 = DIRECTION ( 'NONE',  ( 8.911056267098788616E-18, 1.998401444326210262E-15, 1.000000000000000000 ) ) ;
#12027 = CARTESIAN_POINT ( 'NONE',  ( -57.16110402867079898, 11.90787760832819941, 3.218044905330409686E-15 ) ) ;
#12028 = PERSON_AND_ORGANIZATION_ROLE ( 'creator' ) ;
#12029 = ORIENTED_EDGE ( 'NONE', *, *, #13008, .T. ) ;
#12030 = CARTESIAN_POINT ( 'NONE',  ( 30.84445860938240003, -2.459566909556700320, -17.25000000000040146 ) ) ;
#12031 = CARTESIAN_POINT ( 'NONE',  ( -25.64161990512560152, 6.365892616704869944, 2.500000000000000000 ) ) ;
#12032 = EDGE_LOOP ( 'NONE', ( #9187, #15734 ) ) ;
#12033 = EDGE_CURVE ( 'NONE', #22020, #965, #12091, .T. ) ;
#12034 = EDGE_CURVE ( 'NONE', #21214, #16249, #19644, .T. ) ;
#12035 = DIRECTION ( 'NONE',  ( -1.138590270679734009E-14, -2.220446049251240387E-15, -1.000000000000000000 ) ) ;
#12036 = DIRECTION ( 'NONE',  ( -0.8633955506089426857, -0.5045276238113038936, -2.575384811085907648E-17 ) ) ;
#12037 = SHAPE_REPRESENTATION ( '1602p_c_18', ( #12739 ), #20713 ) ;
#12038 = LINE ( 'NONE', #15572, #16785 ) ;
#12039 = ORIENTED_EDGE ( 'NONE', *, *, #16620, .F. ) ;
#12040 = CARTESIAN_POINT ( 'NONE',  ( 118.5310588935630136, -6.697506338400830650, -19.59999999999999787 ) ) ;
#12041 = PERSON_AND_ORGANIZATION ( #11966, #8758 ) ;
#12042 = AXIS2_PLACEMENT_3D ( 'NONE', #8529, #23092, #14210 ) ;
#12043 = ORIENTED_EDGE ( 'NONE', *, *, #14333, .F. ) ;
#12044 = EDGE_LOOP ( 'NONE', ( #20995, #7631, #5542, #6439 ) ) ;
#12045 = LINE ( 'NONE', #11810, #13037 ) ;
#12046 = AXIS2_PLACEMENT_3D ( 'NONE', #12914, #2100, #18035 ) ;
#12047 = DIRECTION ( 'NONE',  ( 6.281952996264339472E-17, 4.969341027148640384E-15, 1.000000000000000000 ) ) ;
#12048 = VECTOR ( 'NONE', #9416, 999.9999999999998863 ) ;
#12049 = FACE_OUTER_BOUND ( 'NONE', #8392, .T. ) ;
#12050 = APPLICATION_PROTOCOL_DEFINITION ( 'international standard', 'config_control_design', 1994, #2142 ) ;
#12051 = CARTESIAN_POINT ( 'NONE',  ( 39.67523673029199927, 5.313293424922040487, -15.90000000000000036 ) ) ;
#12052 = CARTESIAN_POINT ( 'NONE',  ( -20.11411981943522775, 20.45469521730081652, 5.000000000004466649 ) ) ;
#12053 = APPROVAL_STATUS ( 'not_yet_approved' ) ;
#12054 = DIRECTION ( 'NONE',  ( 1.138590270679730064E-14, 2.220446049251240387E-15, 1.000000000000000000 ) ) ;
#12055 = EDGE_CURVE ( 'NONE', #11110, #3632, #21319, .T. ) ;
#12056 = AXIS2_PLACEMENT_3D ( 'NONE', #16636, #18806, #717 ) ;
#12057 = FACE_OUTER_BOUND ( 'NONE', #7868, .T. ) ;
#12058 = COORDINATED_UNIVERSAL_TIME_OFFSET ( 0, 0, .AHEAD. ) ;
#12059 = CIRCLE ( 'NONE', #1417, 3.750000000000000000 ) ;
#12060 = CARTESIAN_POINT ( 'NONE',  ( 36.07092311366584880, 11.78608357701223852, 8.759424124907040365 ) ) ;
#12061 = CARTESIAN_POINT ( 'NONE',  ( 34.88044566782581057, 28.44271146055880806, -13.00000000000030020 ) ) ;
#12062 = EDGE_CURVE ( 'NONE', #9018, #15793, #15095, .T. ) ;
#12063 = CARTESIAN_POINT ( 'NONE',  ( 5.000000000000000000, -31.09999999999999787, -21.50000000000000000 ) ) ;
#12064 = DIRECTION ( 'NONE',  ( 0.9999862922474493931, 0.005235963827110170880, 0.000000000000000000 ) ) ;
#12065 = EDGE_CURVE ( 'NONE', #3898, #10218, #3159, .T. ) ;
#12066 = VECTOR ( 'NONE', #11597, 1000.000000000000114 ) ;
#12067 = LINE ( 'NONE', #1099, #16373 ) ;
#12068 = ORIENTED_EDGE ( 'NONE', *, *, #1712, .T. ) ;
#12069 =( REPRESENTATION_RELATIONSHIP ('NONE','NONE', #18771, #18121 ) REPRESENTATION_RELATIONSHIP_WITH_TRANSFORMATION ( #20930 )SHAPE_REPRESENTATION_RELATIONSHIP( ) );
#12070 = CARTESIAN_POINT ( 'NONE',  ( 58.49563186522070168, 17.70675969991889787, 10.74537999999999904 ) ) ;
#12071 = ORIENTED_EDGE ( 'NONE', *, *, #23113, .F. ) ;
#12072 = EDGE_LOOP ( 'NONE', ( #22925, #4155 ) ) ;
#12073 = DIRECTION ( 'NONE',  ( -1.000000000000000000, 1.982541115402065307E-15, 0.000000000000000000 ) ) ;
#12074 = CARTESIAN_POINT ( 'NONE',  ( -19.99999998334471840, -22.50000000000000000, 4.549393491468339877E-12 ) ) ;
#12075 = AXIS2_PLACEMENT_3D ( 'NONE', #580, #11552, #7838 ) ;
#12076 = EDGE_LOOP ( 'NONE', ( #5845, #13136, #19857, #16979, #9449, #1858, #5295, #6370, #22311, #225, #4725 ) ) ;
#12077 = DIRECTION ( 'NONE',  ( 6.123237831918409167E-17, -1.616838880122404932E-30, -1.000000000000000000 ) ) ;
#12078 = VECTOR ( 'NONE', #8627, 1000.000000000000000 ) ;
#12079 = ORIENTED_EDGE ( 'NONE', *, *, #2605, .F. ) ;
#12080 = AXIS2_PLACEMENT_3D ( 'NONE', #15240, #10153, #19280 ) ;
#12081 = CARTESIAN_POINT ( 'NONE',  ( 114.6071564266699880, -22.31351932764730250, 13.00000000000000000 ) ) ;
#12082 = AXIS2_PLACEMENT_3D ( 'NONE', #9563, #15008, #13002 ) ;
#12083 = PERSON_AND_ORGANIZATION ( #11966, #8758 ) ;
#12084 = CARTESIAN_POINT ( 'NONE',  ( 33.95095283150600807, -0.6266201978617900181, 13.00000000000019895 ) ) ;
#12085 = COORDINATED_UNIVERSAL_TIME_OFFSET ( 0, 0, .AHEAD. ) ;
#12086 =( LENGTH_UNIT ( ) NAMED_UNIT ( * ) SI_UNIT ( .MILLI., .METRE. ) );
#12087 = CIRCLE ( 'NONE', #13208, 4.999999999999997335 ) ;
#12088 = FACE_OUTER_BOUND ( 'NONE', #11514, .T. ) ;
#12089 = PRODUCT_DEFINITION ( 'UNKNOWN', '', #3463, #18454 ) ;
#12090 = CARTESIAN_POINT ( 'NONE',  ( 39.27359436029429673, 22.26288585089429972, 13.00000000000000000 ) ) ;
#12091 = CIRCLE ( 'NONE', #12825, 2.699999999999998845 ) ;
#12092 = DIRECTION ( 'NONE',  ( 0.9730401042858036753, -0.2306359803922028995, -5.959266323858677443E-17 ) ) ;
#12093 = ORIENTED_EDGE ( 'NONE', *, *, #8199, .T. ) ;
#12094 = DIRECTION ( 'NONE',  ( -1.000000000000000000, 0.000000000000000000, -1.304396158928240120E-15 ) ) ;
#12095 = DESIGN_CONTEXT ( 'detailed design', #11435, 'design' ) ;
#12096 = CARTESIAN_POINT ( 'NONE',  ( 31.01827548281339375, -2.500766059351137827, -11.00000000000039435 ) ) ;
#12097 = AXIS2_PLACEMENT_3D ( 'NONE', #22591, #13579, #2782 ) ;
#12098 = VERTEX_POINT ( 'NONE', #11852 ) ;
#12099 = CARTESIAN_POINT ( 'NONE',  ( -22.99995202268987171, -0.1204285676208968203, -8.616475246431379602E-14 ) ) ;
#12100 = CARTESIAN_POINT ( 'NONE',  ( -26.75617730459320143, 6.359992804688680224, 9.266501092714649290E-14 ) ) ;
#12101 = SECURITY_CLASSIFICATION_LEVEL ( 'unclassified' ) ;
#12102 = DIRECTION ( 'NONE',  ( 1.000000000000000000, 0.000000000000000000, 1.480297366166879989E-16 ) ) ;
#12103 = EDGE_LOOP ( 'NONE', ( #13228, #10484, #22599, #5615, #5638 ) ) ;
#12104 = EDGE_LOOP ( 'NONE', ( #8068, #9636 ) ) ;
#12105 = CALENDAR_DATE ( 2026, 31, 10 ) ;
#12106 = FACE_OUTER_BOUND ( 'NONE', #10957, .T. ) ;
#12107 = ADVANCED_FACE ( 'NONE', ( #898 ), #23083, .T. ) ;
#12108 = ORIENTED_EDGE ( 'NONE', *, *, #11437, .F. ) ;
#12109 = CARTESIAN_POINT ( 'NONE',  ( -17.47493720815359808, 28.95208920939580111, -6.749999999996149747 ) ) ;
#12110 = PERSON_AND_ORGANIZATION ( #11966, #8758 ) ;
#12111 = VECTOR ( 'NONE', #21810, 1000.000000000000227 ) ;
#12112 = CARTESIAN_POINT ( 'NONE',  ( 0.03403376487640559500, -6.499910899608420500, -2.500000000000090150 ) ) ;
#12113 = CARTESIAN_POINT ( 'NONE',  ( -12.50000000434450165, 26.95208919326699970, -7.999999999997280398 ) ) ;
#12114 = EDGE_LOOP ( 'NONE', ( #14232, #17664, #2226, #11393 ) ) ;
#12115 = EDGE_LOOP ( 'NONE', ( #11085, #8467, #22435, #9004 ) ) ;
#12116 = CARTESIAN_POINT ( 'NONE',  ( -62.73971250800079957, -25.32895006819559924, -5.000000000000000000 ) ) ;
#12117 = DIRECTION ( 'NONE',  ( 0.000000000000000000, -1.000000000000000000, 2.081668171172169697E-15 ) ) ;
#12118 = ORIENTED_EDGE ( 'NONE', *, *, #9353, .T. ) ;
#12119 = CARTESIAN_POINT ( 'NONE',  ( 27.54697342219713718, -5.531877349647827735, 13.00000000000019895 ) ) ;
#12120 = PLANE ( 'NONE',  #22528 ) ;
#12121 = CARTESIAN_POINT ( 'NONE',  ( 33.72726576586484981, 23.57751093913000062, 12.99999999999979927 ) ) ;
#12122 = EDGE_LOOP ( 'NONE', ( #6832, #7074 ) ) ;
#12123 = VERTEX_POINT ( 'NONE', #8274 ) ;
#12124 = DIRECTION ( 'NONE',  ( 1.213490492418610097E-15, 4.861311874477940294E-15, 1.000000000000000000 ) ) ;
#12125 = VERTEX_POINT ( 'NONE', #15385 ) ;
#12126 = PERSON_AND_ORGANIZATION ( #11966, #8758 ) ;
#12127 = EDGE_CURVE ( 'NONE', #16276, #2591, #19658, .T. ) ;
#12128 = ORIENTED_EDGE ( 'NONE', *, *, #13624, .F. ) ;
#12129 = EDGE_LOOP ( 'NONE', ( #10575, #5557, #3630, #4159 ) ) ;
#12130 = DIRECTION ( 'NONE',  ( -0.9730401042858036753, 0.2306359803922028995, -2.740969466505749537E-16 ) ) ;
#12131 = PERSON_AND_ORGANIZATION_ROLE ( 'classification_officer' ) ;
#12132 = AXIS2_PLACEMENT_3D ( 'NONE', #14158, #4667, #17615 ) ;
#12133 = CC_DESIGN_DATE_AND_TIME_ASSIGNMENT ( #17652, #22615, ( #1966 ) ) ;
#12134 = CARTESIAN_POINT ( 'NONE',  ( -11.24263882182209962, 20.87636639668270178, 2.500000000000000000 ) ) ;
#12135 = EDGE_CURVE ( 'NONE', #290, #9398, #20846, .T. ) ;
#12136 = EDGE_CURVE ( 'NONE', #14652, #17862, #3350, .T. ) ;
#12137 = DIRECTION ( 'NONE',  ( -0.9730401042858023430, 0.2306359803922080620, 5.959266323858944916E-17 ) ) ;
#12138 = COORDINATED_UNIVERSAL_TIME_OFFSET ( 0, 0, .AHEAD. ) ;
#12139 = PRODUCT_DEFINITION_SHAPE ( 'NONE', 'NONE',  #13468 ) ;
#12140 = ORIENTED_EDGE ( 'NONE', *, *, #7073, .F. ) ;
#12141 = LOCAL_TIME ( 14, 11, 27.00000000000000000, #23371 ) ;
#12142 = DIRECTION ( 'NONE',  ( 0.005235963827108352890, -0.9999862922474493931, -5.936218956694023463E-19 ) ) ;
#12143 = CIRCLE ( 'NONE', #9466, 2.499999999999998224 ) ;
#12144 = LINE ( 'NONE', #15698, #10924 ) ;
#12145 = EDGE_LOOP ( 'NONE', ( #5697, #21971, #11722, #1900, #6774, #6407, #22442, #20765 ) ) ;
#12146 = CARTESIAN_POINT ( 'NONE',  ( 28.89837840081079889, -1.998294948772166180, 8.750000000000198952 ) ) ;
#12147 = DIRECTION ( 'NONE',  ( -0.005235963827121941846, 0.9999862922474492821, 5.936218956651588485E-19 ) ) ;
#12148 = CARTESIAN_POINT ( 'NONE',  ( 28.87791045744280183, 0.08327042291979450117, -13.50000000000040146 ) ) ;
#12149 = ORIENTED_EDGE ( 'NONE', *, *, #9260, .F. ) ;
#12150 = CIRCLE ( 'NONE', #4215, 2.499999999999999112 ) ;
#12151 = DIRECTION ( 'NONE',  ( -0.9730401042858024541, 0.2306359803922080898, 5.959266323858942451E-17 ) ) ;
#12152 = APPROVAL_DATE_TIME ( #1195, #10128 ) ;
#12153 = ADVANCED_FACE ( 'NONE', ( #1357 ), #1244, .T. ) ;
#12154 = ORIENTED_EDGE ( 'NONE', *, *, #21966, .T. ) ;
#12155 = ORIENTED_EDGE ( 'NONE', *, *, #1369, .T. ) ;
#12156 = CARTESIAN_POINT ( 'NONE',  ( -20.00000001665528160, -17.50000000000000000, 4.538291268782600698E-12 ) ) ;
#12157 = DIRECTION ( 'NONE',  ( 0.000000000000000000, 0.000000000000000000, 1.000000000000000000 ) ) ;
#12158 = CARTESIAN_POINT ( 'NONE',  ( 34.89491389100820129, 23.30074776265920278, 17.25000000000000000 ) ) ;
#12159 = DATE_TIME_ROLE ( 'creation_date' ) ;
#12160 = DIRECTION ( 'NONE',  ( -0.005235963827104182615, 0.9999862922474495042, 7.400535959114223454E-19 ) ) ;
#12161 = APPROVAL ( #15685, 'UNSPECIFIED' ) ;
#12162 = CC_DESIGN_SECURITY_CLASSIFICATION ( #9941, ( #7231 ) ) ;
#12163 = CC_DESIGN_PERSON_AND_ORGANIZATION_ASSIGNMENT ( #17963, #5582, ( #6084 ) ) ;
#12164 = DIRECTION ( 'NONE',  ( 0.9730401042858037863, -0.2306359803922024276, -5.958148513035918094E-17 ) ) ;
#12165 = AXIS2_PLACEMENT_3D ( 'NONE', #10064, #4463, #1116 ) ;
#12166 =( GEOMETRIC_REPRESENTATION_CONTEXT ( 3 ) GLOBAL_UNCERTAINTY_ASSIGNED_CONTEXT ( ( #10631 ) ) GLOBAL_UNIT_ASSIGNED_CONTEXT ( ( #237, #15094, #22325 ) ) REPRESENTATION_CONTEXT ( 'NONE', 'WORKASPACE' ) );
#12167 = CIRCLE ( 'NONE', #15172, 2.500000000000001776 ) ;
#12168 = CARTESIAN_POINT ( 'NONE',  ( -30.72441677844230057, -6.660963241697680282, -5.500000000000089706 ) ) ;
#12169 = ADVANCED_FACE ( 'NONE', ( #14077 ), #19195, .T. ) ;
#12170 = EDGE_CURVE ( 'NONE', #4999, #16244, #23110, .T. ) ;
#12171 = CC_DESIGN_DATE_AND_TIME_ASSIGNMENT ( #20057, #18415, ( #4882 ) ) ;
#12172 = LINE ( 'NONE', #17144, #9813 ) ;
#12173 = APPLICATION_PROTOCOL_DEFINITION ( 'international standard', 'config_control_design', 1994, #4269 ) ;
#12174 =( BOUNDED_CURVE ( )  B_SPLINE_CURVE ( 2, ( #5809, #20295, #4020 ),
 .UNSPECIFIED., .F., .F. ) 
 B_SPLINE_CURVE_WITH_KNOTS ( ( 3, 3 ),
 ( 0.000000000000000000, 0.2336872276155859962 ),
 .UNSPECIFIED. ) 
 CURVE ( )  GEOMETRIC_REPRESENTATION_ITEM ( )  RATIONAL_B_SPLINE_CURVE ( ( 1.000000000000000000, 1.154700538379259900, 1.000000000000000000 ) ) 
 REPRESENTATION_ITEM ( '' )  );
#12175 = VECTOR ( 'NONE', #23401, 1000.000000000000000 ) ;
#12176 = CARTESIAN_POINT ( 'NONE',  ( 35.38564976618402369, 7.713890031107105472, 8.762651562745531919 ) ) ;
#12177 = DIRECTION ( 'NONE',  ( -3.099353312215989243E-62, 0.000000000000000000, 1.000000000000000000 ) ) ;
#12178 = CARTESIAN_POINT ( 'NONE',  ( 37.46113131852679601, -4.027891576221660053, -13.00000000000000000 ) ) ;
#12179 = CC_DESIGN_SECURITY_CLASSIFICATION ( #20495, ( #20866 ) ) ;
#12180 = FACE_OUTER_BOUND ( 'NONE', #21554, .T. ) ;
#12181 = CARTESIAN_POINT ( 'NONE',  ( -59.85533902005759899, -24.86725927682059734, 5.000000000000000000 ) ) ;
#12182 = ORIENTED_EDGE ( 'NONE', *, *, #67, .T. ) ;
#12183 = DIRECTION ( 'NONE',  ( 1.000000000000000000, -2.611676738638919574E-15, 0.000000000000000000 ) ) ;
#12184 = EDGE_CURVE ( 'NONE', #8528, #15954, #18505, .T. ) ;
#12185 = ORIENTED_EDGE ( 'NONE', *, *, #12315, .T. ) ;
#12186 = CARTESIAN_POINT ( 'NONE',  ( -12.99532053203719961, 13.48190178978399878, -2.500000000000000000 ) ) ;
#12187 = PLANE ( 'NONE',  #10997 ) ;
#12188 = ORIENTED_EDGE ( 'NONE', *, *, #1280, .T. ) ;
#12189 = AXIS2_PLACEMENT_3D ( 'NONE', #20282, #1422, #8686 ) ;
#12190 = DIRECTION ( 'NONE',  ( -0.2306359803921919083, -0.9730401042858062288, 2.222614453595293935E-13 ) ) ;
#12191 = EDGE_CURVE ( 'NONE', #21354, #20679, #7136, .T. ) ;
#12192 = EDGE_LOOP ( 'NONE', ( #19885, #4222, #10432, #19034, #19298 ) ) ;
#12193 = FACE_OUTER_BOUND ( 'NONE', #15068, .T. ) ;
#12194 = PERSON_AND_ORGANIZATION_ROLE ( 'classification_officer' ) ;
#12195 = CARTESIAN_POINT ( 'NONE',  ( -30.15694676875160241, 9.287188980624568657, 5.000000000000000000 ) ) ;
#12196 = ADVANCED_FACE ( 'NONE', ( #19310 ), #19425, .T. ) ;
#12197 = CC_DESIGN_APPROVAL ( #21860, ( #13468 ) ) ;
#12198 = EDGE_CURVE ( 'NONE', #12644, #15787, #1524, .T. ) ;
#12199 = COORDINATED_UNIVERSAL_TIME_OFFSET ( 0, 0, .AHEAD. ) ;
#12200 = SHAPE_REPRESENTATION_RELATIONSHIP ( 'NONE' , 'NONE' ,  #4731, #15041 ) ;
#12201 = APPROVAL_PERSON_ORGANIZATION ( #20532, #16346, #13767 ) ;
#12202 = CARTESIAN_POINT ( 'NONE',  ( -19.99999998167723803, -22.75000000000000000, 8.500000000004558132 ) ) ;
#12203 = CIRCLE ( 'NONE', #17111, 2.500000000000000888 ) ;
#12204 = CARTESIAN_POINT ( 'NONE',  ( -11.00000000000000000, -27.34999999999999787, 6.250000000000000000 ) ) ;
#12205 = DIRECTION ( 'NONE',  ( 0.000000000000000000, 0.000000000000000000, 1.000000000000000000 ) ) ;
#12206 = LOCAL_TIME ( 14, 11, 27.00000000000000000, #9490 ) ;
#12207 = FACE_OUTER_BOUND ( 'NONE', #17198, .T. ) ;
#12208 = ORIENTED_EDGE ( 'NONE', *, *, #17900, .F. ) ;
#12209 = PLANE ( 'NONE',  #15083 ) ;
#12210 = ADVANCED_BREP_SHAPE_REPRESENTATION ( '', ( #1279, #12739 ), #13514 ) ;
#12211 = LINE ( 'NONE', #15753, #8020 ) ;
#12212 = ORIENTED_EDGE ( 'NONE', *, *, #15055, .T. ) ;
#12213 = CARTESIAN_POINT ( 'NONE',  ( 36.07092311366589854, 11.78608357701213905, -8.759424124907058129 ) ) ;
#12214 = CARTESIAN_POINT ( 'NONE',  ( 5.750000000000129674, -20.33108891324529921, 2.500000000000000000 ) ) ;
#12215 = ORIENTED_EDGE ( 'NONE', *, *, #1179, .T. ) ;
#12216 = LOCAL_TIME ( 14, 11, 27.00000000000000000, #16331 ) ;
#12217 = CALENDAR_DATE ( 2026, 31, 10 ) ;
#12218 = DIRECTION ( 'NONE',  ( -0.9999862922474493931, -0.005235963827116132258, 1.187304881134280213E-16 ) ) ;
#12219 = LOCAL_TIME ( 14, 11, 27.00000000000000000, #8597 ) ;
#12220 = ORIENTED_EDGE ( 'NONE', *, *, #14700, .T. ) ;
#12221 = ORIENTED_EDGE ( 'NONE', *, *, #17575, .F. ) ;
#12222 = AXIS2_PLACEMENT_3D ( 'NONE', #17086, #17223, #21115 ) ;
#12223 = APPROVAL_ROLE ( '' ) ;
#12224 = DIRECTION ( 'NONE',  ( 0.000000000000000000, 0.000000000000000000, -1.000000000000000000 ) ) ;
#12225 = ORIENTED_EDGE ( 'NONE', *, *, #16957, .F. ) ;
#12226 = LINE ( 'NONE', #18667, #4368 ) ;
#12227 = SECURITY_CLASSIFICATION ( '', '', #11883 ) ;
#12228 = APPLICATION_PROTOCOL_DEFINITION ( 'international standard', 'config_control_design', 1994, #3996 ) ;
#12229 = PERSON_AND_ORGANIZATION_ROLE ( 'classification_officer' ) ;
#12230 = CARTESIAN_POINT ( 'NONE',  ( -12.50000000434259917, 26.95208919326709918, 5.500000000004369838 ) ) ;
#12231 = LOCAL_TIME ( 14, 11, 27.00000000000000000, #16741 ) ;
#12232 = DIRECTION ( 'NONE',  ( -1.000000000000000000, 0.000000000000000000, 0.000000000000000000 ) ) ;
#12233 = CIRCLE ( 'NONE', #17526, 3.499999999999999556 ) ;
#12234 = ORIENTED_EDGE ( 'NONE', *, *, #9494, .F. ) ;
#12235 = EDGE_CURVE ( 'NONE', #19161, #3952, #2812, .T. ) ;
#12236 = EDGE_LOOP ( 'NONE', ( #9213, #10458, #12240, #12337 ) ) ;
#12237 = CC_DESIGN_SECURITY_CLASSIFICATION ( #13727, ( #23500 ) ) ;
#12238 = CARTESIAN_POINT ( 'NONE',  ( -20.00000002062990490, 25.45208919256889857, -7.999999999995553779 ) ) ;
#12239 = DIRECTION ( 'NONE',  ( -4.028143194477080210E-16, -2.054129435991050111E-15, -1.000000000000000000 ) ) ;
#12240 = ORIENTED_EDGE ( 'NONE', *, *, #7656, .T. ) ;
#12241 = AXIS2_PLACEMENT_3D ( 'NONE', #3229, #12047, #15711 ) ;
#12242 = FACE_OUTER_BOUND ( 'NONE', #4367, .T. ) ;
#12243 = DIRECTION ( 'NONE',  ( 0.000000000000000000, 0.000000000000000000, -1.000000000000000000 ) ) ;
#12244 = ORIENTED_EDGE ( 'NONE', *, *, #21471, .T. ) ;
#12245 = ORIENTED_EDGE ( 'NONE', *, *, #19093, .T. ) ;
#12246 = DIRECTION ( 'NONE',  ( -0.9730401042858024541, 0.2306359803922080898, 5.959266323858942451E-17 ) ) ;
#12247 = ORIENTED_EDGE ( 'NONE', *, *, #16491, .F. ) ;
#12248 = CALENDAR_DATE ( 2026, 31, 10 ) ;
#12249 = CC_DESIGN_APPROVAL ( #12161, ( #5001 ) ) ;
#12250 = ORIENTED_EDGE ( 'NONE', *, *, #83, .F. ) ;
#12251 = VERTEX_POINT ( 'NONE', #8387 ) ;
#12252 = CARTESIAN_POINT ( 'NONE',  ( 33.37436288052550282, -3.059220458576299873, 13.00000000000019895 ) ) ;
#12253 = PERSON_AND_ORGANIZATION ( #11966, #8758 ) ;
#12254 = CIRCLE ( 'NONE', #11513, 3.500000000000001332 ) ;
#12255 = VECTOR ( 'NONE', #1228, 1000.000000000000000 ) ;
#12256 = CIRCLE ( 'NONE', #6539, 2.500000000000000000 ) ;
#12257 = CARTESIAN_POINT ( 'NONE',  ( 113.2320189960273495, -11.71050705297551531, 3.443204550052153714E-14 ) ) ;
#12258 = AXIS2_PLACEMENT_3D ( 'NONE', #6799, #10253, #3224 ) ;
#12260 = CIRCLE ( 'NONE', #85, 3.499999999999999556 ) ;
#12259 = DIRECTION ( 'NONE',  ( 0.000000000000000000, 0.000000000000000000, -1.000000000000000000 ) ) ;
#12261 = EDGE_CURVE ( 'NONE', #12703, #21124, #13731, .T. ) ;
#12262 = DATE_TIME_ROLE ( 'classification_date' ) ;
#12263 = LOCAL_TIME ( 14, 11, 27.00000000000000000, #5455 ) ;
#12264 = ORIENTED_EDGE ( 'NONE', *, *, #5899, .T. ) ;
#12265 = DIRECTION ( 'NONE',  ( 0.000000000000000000, 0.000000000000000000, 1.000000000000000000 ) ) ;
#12266 = AXIS2_PLACEMENT_3D ( 'NONE', #13078, #18541, #22195 ) ;
#12267 = DIRECTION ( 'NONE',  ( 0.9730401042858036753, -0.2306359803922031493, -5.959266323858673745E-17 ) ) ;
#12268 = ORIENTED_EDGE ( 'NONE', *, *, #12007, .T. ) ;
#12269 = AXIS2_PLACEMENT_3D ( 'NONE', #2284, #11698, #15110 ) ;
#12270 = APPROVAL ( #4949, 'UNKNOWN' ) ;
#12271 = LINE ( 'NONE', #23149, #20383 ) ;
#12272 = AXIS2_PLACEMENT_3D ( 'NONE', #11372, #9100, #11017 ) ;
#12273 = CARTESIAN_POINT ( 'NONE',  ( 33.37436288052550282, -3.059220458576419777, -13.00000000000039968 ) ) ;
#12274 = LINE ( 'NONE', #21041, #17564 ) ;
#12275 = ORIENTED_EDGE ( 'NONE', *, *, #22296, .F. ) ;
#12276 = DIRECTION ( 'NONE',  ( -0.2306359803922094498, -0.9730401042858020100, 1.412237191019847142E-17 ) ) ;
#12277 = EDGE_CURVE ( 'NONE', #7064, #15418, #3030, .T. ) ;
#12278 = ADVANCED_FACE ( 'NONE', ( #1593 ), #17876, .T. ) ;
#12279 = DATE_AND_TIME ( #19268, #14443 ) ;
#12280 = VERTEX_POINT ( 'NONE', #6976 ) ;
#12281 = ORIENTED_EDGE ( 'NONE', *, *, #17073, .T. ) ;
#12282 = DIRECTION ( 'NONE',  ( -0.8823529412199823119, 0.4705882352125332901, 1.992040791580033901E-13 ) ) ;
#12283 = FACE_OUTER_BOUND ( 'NONE', #5489, .T. ) ;
#12284 = DIRECTION ( 'NONE',  ( -0.9730401042858036753, 0.2306359803922028995, 5.959266323858677443E-17 ) ) ;
#12285 = APPROVAL_STATUS ( 'not_yet_approved' ) ;
#12286 = CIRCLE ( 'NONE', #22147, 49.22658835543909817 ) ;
#12287 = CARTESIAN_POINT ( 'NONE',  ( 36.76586756491560237, 21.07724224331889573, 13.99999999999999822 ) ) ;
#12288 = APPROVAL_PERSON_ORGANIZATION ( #17292, #18224, #22967 ) ;
#12289 = CARTESIAN_POINT ( 'NONE',  ( -55.91259579215963527, 7.707349321388981878, -7.200000000000000178 ) ) ;
#12290 = VECTOR ( 'NONE', #1322, 1000.000000000000000 ) ;
#12291 = CIRCLE ( 'NONE', #22873, 2.066999999999999282 ) ;
#12292 =( LENGTH_UNIT ( ) NAMED_UNIT ( * ) SI_UNIT ( .MILLI., .METRE. ) );
#12293 = ORIENTED_EDGE ( 'NONE', *, *, #12325, .F. ) ;
#12294 = CARTESIAN_POINT ( 'NONE',  ( 5.750000000000129674, -20.33108891324529921, 5.000000000000000000 ) ) ;
#12295 = ADVANCED_FACE ( 'NONE', ( #8971 ), #10648, .F. ) ;
#12296 = SHAPE_DEFINITION_REPRESENTATION ( #18025, #10092 ) ;
#12297 = CARTESIAN_POINT ( 'NONE',  ( 37.01658734137052420, 11.28063437484922815, 8.819862741542941365 ) ) ;
#12298 = VECTOR ( 'NONE', #2139, 1000.000000000000227 ) ;
#12299 = DIRECTION ( 'NONE',  ( 1.734723475976802677E-14, 4.336808689942006376E-14, 1.000000000000000000 ) ) ;
#12300 = APPROVAL ( #6506, 'UNSPECIFIED' ) ;
#12301 = DIRECTION ( 'NONE',  ( 0.005235963827063078342, -0.9999862922474496152, 2.538154295128170621E-14 ) ) ;
#12302 = CIRCLE ( 'NONE', #9635, 2.499999999999999112 ) ;
#12303 = CARTESIAN_POINT ( 'NONE',  ( 39.76749112244880280, 5.702509466636339397, 15.50000000000000000 ) ) ;
#12304 = APPROVAL ( #4602, 'UNSPECIFIED' ) ;
#12305 = CARTESIAN_POINT ( 'NONE',  ( -20.00000000000000000, -17.50000000000000000, 5.000000000004554579 ) ) ;
#12306 = VERTEX_POINT ( 'NONE', #159 ) ;
#12307 = AXIS2_PLACEMENT_3D ( 'NONE', #19604, #17607, #14256 ) ;
#12308 = LINE ( 'NONE', #1224, #20210 ) ;
#12309 = EDGE_CURVE ( 'NONE', #6828, #15056, #8653, .T. ) ;
#12310 = EDGE_CURVE ( 'NONE', #9901, #3862, #22753, .T. ) ;
#12311 = ADVANCED_FACE ( 'NONE', ( #23438 ), #20007, .F. ) ;
#12312 = VERTEX_POINT ( 'NONE', #7192 ) ;
#12313 = CARTESIAN_POINT ( 'NONE',  ( 33.94234173009040489, 21.44981837135929936, 13.50000000000000000 ) ) ;
#12314 = CYLINDRICAL_SURFACE ( 'NONE', #12541, 2.066999999999998838 ) ;
#12315 = EDGE_CURVE ( 'NONE', #6349, #21144, #14201, .T. ) ;
#12316 = EDGE_LOOP ( 'NONE', ( #20512, #10701 ) ) ;
#12317 = DIRECTION ( 'NONE',  ( 2.670035496199930325E-15, 1.152311220646620054E-14, -1.000000000000000000 ) ) ;
#12318 = ORIENTED_EDGE ( 'NONE', *, *, #9288, .T. ) ;
#12319 = CARTESIAN_POINT ( 'NONE',  ( 39.27359436029429673, 22.26288585089429972, 13.00000000000000000 ) ) ;
#12320 = COORDINATED_UNIVERSAL_TIME_OFFSET ( 0, 0, .AHEAD. ) ;
#12321 = CARTESIAN_POINT ( 'NONE',  ( 37.37362508103680625, 25.08661566644150298, -13.00000000000049916 ) ) ;
#12322 = AXIS2_PLACEMENT_3D ( 'NONE', #5064, #21438, #8276 ) ;
#12323 = CIRCLE ( 'NONE', #5097, 2.066999999999999726 ) ;
#12324 = DIRECTION ( 'NONE',  ( 7.515353331921825981E-30, -5.761557392270000270E-15, 1.000000000000000000 ) ) ;
#12325 = EDGE_CURVE ( 'NONE', #17065, #404, #13201, .T. ) ;
#12326 = DIRECTION ( 'NONE',  ( -2.269700743865589996E-13, -2.220446049247695246E-15, -1.000000000000000000 ) ) ;
#12327 = ADVANCED_FACE ( 'NONE', ( #14420 ), #11000, .F. ) ;
#12328 = DIRECTION ( 'NONE',  ( 1.000000000000000000, 0.000000000000000000, 0.000000000000000000 ) ) ;
#12329 = CARTESIAN_POINT ( 'NONE',  ( -62.93786153767959490, 12.51438117767279934, 3.385904617822409831E-15 ) ) ;
#12330 = VERTEX_POINT ( 'NONE', #12426 ) ;
#12331 = CARTESIAN_POINT ( 'NONE',  ( 6.500000000000000000, -17.30000000000000071, -5.000000000000000000 ) ) ;
#12332 = DIRECTION ( 'NONE',  ( 0.2306359803922029827, 0.9730401042858035643, -4.849856555169146878E-15 ) ) ;
#12333 = VERTEX_POINT ( 'NONE', #3505 ) ;
#12334 = DIRECTION ( 'NONE',  ( -0.9730401042858035643, 0.2306359803922028717, 5.959266323858677443E-17 ) ) ;
#12335 = CARTESIAN_POINT ( 'NONE',  ( -24.50000000000000000, -28.60000000000000142, -21.50000000000000000 ) ) ;
#12336 = EDGE_CURVE ( 'NONE', #4833, #5237, #10569, .T. ) ;
#12338 = EDGE_CURVE ( 'NONE', #19990, #6859, #10942, .T. ) ;
#12337 = ORIENTED_EDGE ( 'NONE', *, *, #11001, .F. ) ;
#12339 = CARTESIAN_POINT ( 'NONE',  ( 35.84667945578014780, -10.83917230622359895, 16.00000000000000000 ) ) ;
#12340 = EDGE_CURVE ( 'NONE', #16889, #22403, #18112, .T. ) ;
#12341 = ORIENTED_EDGE ( 'NONE', *, *, #8732, .T. ) ;
#12342 = ORIENTED_EDGE ( 'NONE', *, *, #21996, .T. ) ;
#12343 = APPLICATION_CONTEXT ( 'configuration controlled 3d designs of mechanical parts and assemblies' ) ;
#12344 = PERSON_AND_ORGANIZATION ( #11966, #8758 ) ;
#12345 = LINE ( 'NONE', #19324, #866 ) ;
#12346 = EDGE_LOOP ( 'NONE', ( #8562, #13383, #2634, #4454 ) ) ;
#12347 = LINE ( 'NONE', #19678, #15464 ) ;
#12348 = DATE_AND_TIME ( #13984, #17561 ) ;
#12349 = APPROVAL_ROLE ( '' ) ;
#12350 = DIRECTION ( 'NONE',  ( -0.9730401042858024541, 0.2306359803922080898, 5.959266323859062013E-17 ) ) ;
#12351 = EDGE_CURVE ( 'NONE', #19229, #15489, #13954, .T. ) ;
#12352 = CIRCLE ( 'NONE', #11980, 2.749999999999999112 ) ;
#12353 = CARTESIAN_POINT ( 'NONE',  ( -20.00000000000000000, -25.00000000000000000, 5.000000000004570566 ) ) ;
#12354 = ORIENTED_EDGE ( 'NONE', *, *, #14333, .T. ) ;
#12355 = ORIENTED_EDGE ( 'NONE', *, *, #2964, .T. ) ;
#12356 = EDGE_CURVE ( 'NONE', #2561, #11172, #12877, .T. ) ;
#12357 = CARTESIAN_POINT ( 'NONE',  ( 49.97703550743810297, 19.72589006657999988, -15.50000000000049916 ) ) ;
#12358 = ORIENTED_EDGE ( 'NONE', *, *, #21765, .T. ) ;
#12359 = EDGE_CURVE ( 'NONE', #22197, #12472, #9797, .T. ) ;
#12360 = CARTESIAN_POINT ( 'NONE',  ( 114.2412296582674429, -24.79605227811687485, 13.00000000000000000 ) ) ;
#12361 = DIRECTION ( 'NONE',  ( 0.9730401042858024541, -0.2306359803922080898, -5.959266323858592394E-17 ) ) ;
#12362 = ORIENTED_EDGE ( 'NONE', *, *, #5172, .F. ) ;
#12363 = ORIENTED_EDGE ( 'NONE', *, *, #18643, .F. ) ;
#12364 = ORIENTED_EDGE ( 'NONE', *, *, #18742, .T. ) ;
#12365 = APPROVAL_ROLE ( '' ) ;
#12366 = ORIENTED_EDGE ( 'NONE', *, *, #16368, .T. ) ;
#12367 = EDGE_LOOP ( 'NONE', ( #10992, #18756, #4720, #1039, #10834 ) ) ;
#12368 = CARTESIAN_POINT ( 'NONE',  ( -19.99999999999999645, -15.00000000000000000, 5.000000000004549250 ) ) ;
#12369 = PERSON_AND_ORGANIZATION_ROLE ( 'creator' ) ;
#12370 = DIRECTION ( 'NONE',  ( -0.1153179901961009640, -0.4865200521429018377, 0.8660254037844385966 ) ) ;
#12371 = CARTESIAN_POINT ( 'NONE',  ( -65.64475015647069256, -21.84411297095480009, 5.000000000000000000 ) ) ;
#12372 = CC_DESIGN_DATE_AND_TIME_ASSIGNMENT ( #15097, #7745, ( #12933 ) ) ;
#12373 = DATE_AND_TIME ( #23271, #4936 ) ;
#12374 = ORIENTED_EDGE ( 'NONE', *, *, #20825, .F. ) ;
#12375 = PLANE ( 'NONE',  #6467 ) ;
#12376 = DIRECTION ( 'NONE',  ( 0.2306359803922101437, 0.9730401042858017879, -4.006172263299087069E-15 ) ) ;
#12377 = VERTEX_POINT ( 'NONE', #14305 ) ;
#12378 = AXIS2_PLACEMENT_3D ( 'NONE', #18285, #7244, #14824 ) ;
#12379 = LINE ( 'NONE', #16041, #3698 ) ;
#12380 = CARTESIAN_POINT ( 'NONE',  ( -26.99999999999959854, -19.33065833018799751, 21.49999999999999289 ) ) ;
#12381 = DIRECTION ( 'NONE',  ( 0.005235963827121942714, -0.9999862922474493931, -2.738609489598291197E-14 ) ) ;
#12382 = VERTEX_POINT ( 'NONE', #9202 ) ;
#12383 = VERTEX_POINT ( 'NONE', #3268 ) ;
#12384 = DIRECTION ( 'NONE',  ( -1.380319151413309694E-18, 2.636191302913840582E-16, -1.000000000000000000 ) ) ;
#12385 = COORDINATED_UNIVERSAL_TIME_OFFSET ( 0, 0, .AHEAD. ) ;
#12386 = VERTEX_POINT ( 'NONE', #1471 ) ;
#12387 = EDGE_LOOP ( 'NONE', ( #9144, #4507, #5339, #5315 ) ) ;
#12388 = PLANE ( 'NONE',  #9962 ) ;
#12389 = DIRECTION ( 'NONE',  ( -1.000000000000000000, 0.000000000000000000, 0.000000000000000000 ) ) ;
#12390 = DIRECTION ( 'NONE',  ( 0.2306359803922080898, 0.9730401042858024541, -2.572202231434325988E-16 ) ) ;
#12391 = APPROVAL_STATUS ( 'not_yet_approved' ) ;
#12392 = DIRECTION ( 'NONE',  ( -0.9080662505684728991, 0.4188265566777199522, -1.051895949684139634E-15 ) ) ;
#12393 = ADVANCED_FACE ( 'NONE', ( #21540 ), #5276, .T. ) ;
#12394 = AXIS2_PLACEMENT_3D ( 'NONE', #4166, #15089, #22322 ) ;
#12395 = LINE ( 'NONE', #15716, #12175 ) ;
#12396 = EDGE_CURVE ( 'NONE', #11640, #9680, #11708, .T. ) ;
#12397 = DIRECTION ( 'NONE',  ( 0.9730401042858035643, -0.2306359803922028717, -5.958148513035547083E-17 ) ) ;
#12398 = APPROVAL_ROLE ( '' ) ;
#12399 = CARTESIAN_POINT ( 'NONE',  ( 62.70840910389689782, 3.348031886875269869, 1.061114750357439988E-14 ) ) ;
#12400 = DIRECTION ( 'NONE',  ( -0.9730401042858022320, 0.2306359803922080343, 5.959266323858941219E-17 ) ) ;
#12401 = CARTESIAN_POINT ( 'NONE',  ( 36.78282996199610722, 11.03463321983590006, 29.25000000000000000 ) ) ;
#12402 = CARTESIAN_POINT ( 'NONE',  ( 41.08211621068439712, 11.24883806106539907, 18.89999999999999858 ) ) ;
#12403 = AXIS2_PLACEMENT_3D ( 'NONE', #13940, #23065, #4686 ) ;
#12404 = AXIS2_PLACEMENT_3D ( 'NONE', #3705, #1566, #5495 ) ;
#12405 = CARTESIAN_POINT ( 'NONE',  ( 35.09747506357100377, 11.43410645592840069, -27.69000000000049866 ) ) ;
#12406 = EDGE_LOOP ( 'NONE', ( #3719, #18042 ) ) ;
#12407 = LINE ( 'NONE', #12070, #23230 ) ;
#12408 = ORIENTED_EDGE ( 'NONE', *, *, #15198, .T. ) ;
#12409 = FACE_OUTER_BOUND ( 'NONE', #18457, .T. ) ;
#12410 = CARTESIAN_POINT ( 'NONE',  ( -25.64161990512560152, 6.365892616704879714, 3.750000000000000000 ) ) ;
#12411 = ORIENTED_EDGE ( 'NONE', *, *, #6003, .F. ) ;
#12412 = CARTESIAN_POINT ( 'NONE',  ( 36.88454136754629786, -6.460491836936129495, -2.999999999999930278 ) ) ;
#12413 = EDGE_CURVE ( 'NONE', #17804, #8958, #3968, .T. ) ;
#12414 = VERTEX_POINT ( 'NONE', #9690 ) ;
#12415 = CARTESIAN_POINT ( 'NONE',  ( 122.4288069621910040, 9.746871424029301068, 13.00000000000000000 ) ) ;
#12416 = CIRCLE ( 'NONE', #19606, 2.749999999999999112 ) ;
#12417 = DATE_AND_TIME ( #19892, #8868 ) ;
#12418 = DIRECTION ( 'NONE',  ( -0.9730401042858024541, 0.2306359803922080898, 5.959266323862942222E-17 ) ) ;
#12419 = CC_DESIGN_DATE_AND_TIME_ASSIGNMENT ( #18705, #381, ( #6978 ) ) ;
#12420 = AXIS2_PLACEMENT_3D ( 'NONE', #14679, #14794, #11503 ) ;
#12421 = CC_DESIGN_PERSON_AND_ORGANIZATION_ASSIGNMENT ( #8002, #15236, ( #3402 ) ) ;
#12422 = VECTOR ( 'NONE', #1768, 1000.000000000000114 ) ;
#12423 = PLANE ( 'NONE',  #2014 ) ;
#12424 = EDGE_CURVE ( 'NONE', #21792, #142, #22236, .T. ) ;
#12425 = ADVANCED_FACE ( 'NONE', ( #20596 ), #20250, .F. ) ;
#12426 = CARTESIAN_POINT ( 'NONE',  ( 120.8143550994449953, 2.935590694028619829, -20.00000000000000000 ) ) ;
#12427 = TOROIDAL_SURFACE ( 'NONE', #8624, 2.700000000000000178, 0.2000000000000000111 ) ;
#12428 = CYLINDRICAL_SURFACE ( 'NONE', #23268, 2.499999999999998668 ) ;
#12429 = ORIENTED_EDGE ( 'NONE', *, *, #20373, .T. ) ;
#12430 = FACE_OUTER_BOUND ( 'NONE', #5900, .T. ) ;
#12431 = ORIENTED_EDGE ( 'NONE', *, *, #12277, .T. ) ;
#12432 = AXIS2_PLACEMENT_3D ( 'NONE', #22217, #1189, #10372 ) ;
#12433 = DIRECTION ( 'NONE',  ( 3.099353312215988811E-62, -1.534091707905539548E-92, -1.000000000000000000 ) ) ;
#12434 = DIRECTION ( 'NONE',  ( -3.099353312215989243E-62, 9.554441540188157279E-93, 1.000000000000000000 ) ) ;
#12435 = VERTEX_POINT ( 'NONE', #7650 ) ;
#12436 = VECTOR ( 'NONE', #6016, 999.9999999999998863 ) ;
#12437 = AXIS2_PLACEMENT_3D ( 'NONE', #9075, #5057, #17761 ) ;
#12438 = FACE_OUTER_BOUND ( 'NONE', #21738, .T. ) ;
#12439 = CONICAL_SURFACE ( 'NONE', #11691, 2.729132938682640397, 1.047197551196598297 ) ;
#12440 = ORIENTED_EDGE ( 'NONE', *, *, #7362, .T. ) ;
#12441 = ORIENTED_EDGE ( 'NONE', *, *, #5469, .F. ) ;
#12442 = CALENDAR_DATE ( 2026, 31, 10 ) ;
#12443 = CARTESIAN_POINT ( 'NONE',  ( -15.00000000000000000, -20.00000000000000000, -2.500000000000000000 ) ) ;
#12444 = ADVANCED_FACE ( 'NONE', ( #4336, #18468 ), #11603, .F. ) ;
#12445 = EDGE_LOOP ( 'NONE', ( #4631, #4162, #2502, #9463, #7523 ) ) ;
#12446 = CARTESIAN_POINT ( 'NONE',  ( -27.00000000000000000, -20.00000000000000000, -2.500000000000000000 ) ) ;
#12447 = CALENDAR_DATE ( 2026, 31, 10 ) ;
#12448 = CONICAL_SURFACE ( 'NONE', #14332, 2.254620000000000513, 0.7853981633974461696 ) ;
#12449 = CC_DESIGN_PERSON_AND_ORGANIZATION_ASSIGNMENT ( #15171, #22412, ( #1997 ) ) ;
#12450 = CC_DESIGN_PERSON_AND_ORGANIZATION_ASSIGNMENT ( #6662, #22666, ( #14070 ) ) ;
#12451 = CONTEXT_DEPENDENT_SHAPE_REPRESENTATION ( #18576, #3994 ) ;
#12452 = AXIS2_PLACEMENT_3D ( 'NONE', #20657, #18654, #2371 ) ;
#12453 = CARTESIAN_POINT ( 'NONE',  ( 36.57467860885130051, 21.71590586959139912, 11.00000000000000000 ) ) ;
#12454 = ADVANCED_FACE ( 'NONE', ( #3970 ), #734, .T. ) ;
#12455 = ADVANCED_FACE ( 'NONE', ( #22128 ), #7888, .F. ) ;
#12456 = VECTOR ( 'NONE', #737, 999.9999999999998863 ) ;
#12457 = AXIS2_PLACEMENT_3D ( 'NONE', #3377, #8866, #10891 ) ;
#12458 = CARTESIAN_POINT ( 'NONE',  ( 29.76326332728156032, 1.650605442299475145, -13.00000000000039968 ) ) ;
#12459 = ORIENTED_EDGE ( 'NONE', *, *, #4204, .T. ) ;
#12460 = LINE ( 'NONE', #2864, #2612 ) ;
#12461 = ORIENTED_EDGE ( 'NONE', *, *, #9384, .F. ) ;
#12462 = DIRECTION ( 'NONE',  ( 0.2306359803922053142, 0.9730401042858028982, 0.000000000000000000 ) ) ;
#12463 = FACE_BOUND ( 'NONE', #3370, .T. ) ;
#12464 = ORIENTED_EDGE ( 'NONE', *, *, #11121, .F. ) ;
#12465 = CARTESIAN_POINT ( 'NONE',  ( -68.69007546624879978, 8.433449002107520798, 2.873144230283079984E-15 ) ) ;
#12466 = DIRECTION ( 'NONE',  ( -0.6880432561069586006, 0.1630842657209347069, -0.7071067811865459074 ) ) ;
#12467 = AXIS2_PLACEMENT_3D ( 'NONE', #17657, #19086, #17299 ) ;
#12468 = EDGE_LOOP ( 'NONE', ( #3653, #14316, #7391, #23455 ) ) ;
#12469 = VERTEX_POINT ( 'NONE', #2434 ) ;
#12470 = DATE_TIME_ROLE ( 'creation_date' ) ;
#12471 = EDGE_CURVE ( 'NONE', #21232, #9241, #5604, .T. ) ;
#12472 = VERTEX_POINT ( 'NONE', #16656 ) ;
#12473 = VERTEX_POINT ( 'NONE', #14891 ) ;
#12474 = CARTESIAN_POINT ( 'NONE',  ( 34.40556712239440174, 8.514986143070938596, -29.25000000000050093 ) ) ;
#12475 = CIRCLE ( 'NONE', #7535, 0.3999999999999998557 ) ;
#12476 = SHAPE_DEFINITION_REPRESENTATION ( #177, #9313 ) ;
#12477 = PLANE ( 'NONE',  #19954 ) ;
#12478 = COORDINATED_UNIVERSAL_TIME_OFFSET ( 0, 0, .AHEAD. ) ;
#12479 = EDGE_CURVE ( 'NONE', #6410, #22407, #16905, .T. ) ;
#12480 = EDGE_CURVE ( 'NONE', #23367, #17438, #1429, .T. ) ;
#12481 =( NAMED_UNIT ( * ) SI_UNIT ( $, .STERADIAN. ) SOLID_ANGLE_UNIT ( ) );
#12482 = DIRECTION ( 'NONE',  ( 0.7806762821592939661, -0.6249356306644248127, -7.632783294297949638E-15 ) ) ;
#12483 = PERSON_AND_ORGANIZATION ( #11966, #8758 ) ;
#12484 = CLOSED_SHELL ( 'NONE', ( #6043, #4642, #485, #3561, #5069, #3139, #21835, #20457, #5533, #8862, #2938, #16016, #7069, #16911, #15741, #18264, #18827 ) ) ;
#12485 = ORIENTED_EDGE ( 'NONE', *, *, #6999, .F. ) ;
#12486 = CARTESIAN_POINT ( 'NONE',  ( -62.84171802989950351, -5.847508446296020068, 7.200000000000000178 ) ) ;
#12487 = DIRECTION ( 'NONE',  ( 0.005235963827117092427, -0.9999862922474493931, -2.636227439667000721E-16 ) ) ;
#12488 = ORIENTED_EDGE ( 'NONE', *, *, #8208, .T. ) ;
#12489 = ADVANCED_BREP_SHAPE_REPRESENTATION ( '', ( #1311, #12739 ), #11790 ) ;
#12490 = DIRECTION ( 'NONE',  ( 1.320147222947482081E-46, -2.155962677239134989E-30, -1.000000000000000000 ) ) ;
#12491 = DIRECTION ( 'NONE',  ( -0.2306359803922028717, -0.9730401042858034533, -4.546664459266603656E-32 ) ) ;
#12492 = DIRECTION ( 'NONE',  ( 0.000000000000000000, -1.000000000000000000, 0.000000000000000000 ) ) ;
#12493 = EDGE_LOOP ( 'NONE', ( #13279, #17949, #8057, #3341 ) ) ;
#12494 = ORIENTED_EDGE ( 'NONE', *, *, #3740, .T. ) ;
#12495 = DIRECTION ( 'NONE',  ( -2.270069654138865127E-15, -1.000000000000000000, 4.574083617919690056E-30 ) ) ;
#12496 = ORIENTED_EDGE ( 'NONE', *, *, #13585, .T. ) ;
#12497 = COORDINATED_UNIVERSAL_TIME_OFFSET ( 0, 0, .AHEAD. ) ;
#12498 = ORIENTED_EDGE ( 'NONE', *, *, #14756, .F. ) ;
#12499 = ORIENTED_EDGE ( 'NONE', *, *, #14116, .F. ) ;
#12500 = CARTESIAN_POINT ( 'NONE',  ( -14.54830929662709949, 0.3367883020382380632, 5.500000000004449774 ) ) ;
#12501 = CARTESIAN_POINT ( 'NONE',  ( 33.27705887009660302, -3.036156860536619817, -13.00000000000000000 ) ) ;
#12502 = CARTESIAN_POINT ( 'NONE',  ( 90.25841307858055984, 13.00434284682846098, -13.00000000000030020 ) ) ;
#12503 = PERSON_AND_ORGANIZATION ( #11966, #8758 ) ;
#12504 = PRODUCT_DEFINITION ( 'UNKNOWN', '', #1510, #12775 ) ;
#12505 = DIRECTION ( 'NONE',  ( 0.1997366180463769070, 0.8426774492125652660, 0.5000000000000003331 ) ) ;
#12506 = LINE ( 'NONE', #19740, #22003 ) ;
#12507 =( REPRESENTATION_RELATIONSHIP ('NONE','NONE', #19303, #488 ) REPRESENTATION_RELATIONSHIP_WITH_TRANSFORMATION ( #9249 )SHAPE_REPRESENTATION_RELATIONSHIP( ) );
#12508 = SHAPE_REPRESENTATION ( '1602p_c_47', ( #12739 ), #15936 ) ;
#12509 = DIRECTION ( 'NONE',  ( 0.000000000000000000, 0.000000000000000000, 1.000000000000000000 ) ) ;
#12510 = APPROVAL_PERSON_ORGANIZATION ( #2777, #17350, #4785 ) ;
#12511 = CIRCLE ( 'NONE', #7948, 2.499999999999999112 ) ;
#12512 = DIRECTION ( 'NONE',  ( -0.005235963827108352890, 0.9999862922474493931, 5.936218956694023463E-19 ) ) ;
#12513 = CALENDAR_DATE ( 2026, 31, 10 ) ;
#12514 = CARTESIAN_POINT ( 'NONE',  ( -20.00000000000000000, -25.00000000000000000, -4.999999999995459632 ) ) ;
#12515 = LINE ( 'NONE', #19748, #11675 ) ;
#12516 = FACE_OUTER_BOUND ( 'NONE', #16495, .T. ) ;
#12517 = ADVANCED_FACE ( 'NONE', ( #271 ), #9437, .F. ) ;
#12518 = DIRECTION ( 'NONE',  ( -0.9730401042858024541, 0.2306359803922080898, 5.959266323859172946E-17 ) ) ;
#12519 = DIRECTION ( 'NONE',  ( 0.000000000000000000, 0.000000000000000000, 1.000000000000000000 ) ) ;
#12520 = ORIENTED_EDGE ( 'NONE', *, *, #20167, .T. ) ;
#12521 = LINE ( 'NONE', #7411, #8447 ) ;
#12522 = UNCERTAINTY_MEASURE_WITH_UNIT (LENGTH_MEASURE( 1.000000000000000082E-05 ), #18441, 'distance_accuracy_value', 'NONE');
#12523 = PRODUCT ( '1602p_c_07', '1602p_c_07', '', ( #12837 ) ) ;
#12524 = ORIENTED_EDGE ( 'NONE', *, *, #7182, .T. ) ;
#12525 = DIRECTION ( 'NONE',  ( -0.9730401042858035643, 0.2306359803922028717, 6.126766849694256332E-17 ) ) ;
#12526 = LINE ( 'NONE', #7416, #22725 ) ;
#12527 = AXIS2_PLACEMENT_3D ( 'NONE', #6470, #15738, #6721 ) ;
#12528 = VERTEX_POINT ( 'NONE', #13121 ) ;
#12529 = CIRCLE ( 'NONE', #14023, 2.500000000000000444 ) ;
#12530 = DIRECTION ( 'NONE',  ( 0.005235963827108352890, -0.9999862922474493931, -2.671135040551771006E-18 ) ) ;
#12531 = ORIENTED_EDGE ( 'NONE', *, *, #5145, .T. ) ;
#12532 = LINE ( 'NONE', #19649, #20754 ) ;
#12533 = PERSON_AND_ORGANIZATION ( #11966, #8758 ) ;
#12534 = DIRECTION ( 'NONE',  ( -0.9730401042858024541, 0.2306359803922080898, 5.959266323858952312E-17 ) ) ;
#12535 = DIRECTION ( 'NONE',  ( -0.9997648975362233292, -0.02168293463497958373, 0.000000000000000000 ) ) ;
#12536 = MECHANICAL_CONTEXT ( 'NONE', #19158, 'mechanical' ) ;
#12537 = CC_DESIGN_APPROVAL ( #17515, ( #4882 ) ) ;
#12538 = AXIS2_PLACEMENT_3D ( 'NONE', #5630, #16435, #12769 ) ;
#12539 = LINE ( 'NONE', #16098, #17243 ) ;
#12540 = DIRECTION ( 'NONE',  ( -0.9730401042858035643, 0.2306359803922028717, 6.126766849694256332E-17 ) ) ;
#12541 = AXIS2_PLACEMENT_3D ( 'NONE', #15958, #3253, #6830 ) ;
#12542 = DIRECTION ( 'NONE',  ( -0.9730401042858024541, 0.2306359803922080898, 5.959266323858942451E-17 ) ) ;
#12543 = ADVANCED_FACE ( 'NONE', ( #6099 ), #9413, .F. ) ;
#12544 = DIRECTION ( 'NONE',  ( -2.270069654138865127E-15, -1.000000000000000000, -4.543838814073030634E-30 ) ) ;
#12545 = VERTEX_POINT ( 'NONE', #9801 ) ;
#12546 = DIRECTION ( 'NONE',  ( -0.2306359803922025109, -0.9730401042858035643, 5.112869192352692394E-15 ) ) ;
#12547 = DIRECTION ( 'NONE',  ( 0.2306359803922032325, 0.9730401042858035643, -1.407521210652540462E-17 ) ) ;
#12548 = CIRCLE ( 'NONE', #16690, 2.500000000000000888 ) ;
#12549 = CC_DESIGN_DATE_AND_TIME_ASSIGNMENT ( #12793, #16459, ( #1558 ) ) ;
#12550 = ORIENTED_EDGE ( 'NONE', *, *, #8964, .T. ) ;
#12551 = COORDINATED_UNIVERSAL_TIME_OFFSET ( 0, 0, .AHEAD. ) ;
#12552 = DIRECTION ( 'NONE',  ( 1.000000000000000000, 9.250482324585361611E-11, -2.269018306577663175E-13 ) ) ;
#12553 = AXIS2_PLACEMENT_3D ( 'NONE', #3116, #23167, #4902 ) ;
#12554 = VERTEX_POINT ( 'NONE', #3843 ) ;
#12555 = EDGE_CURVE ( 'NONE', #15043, #15812, #11124, .T. ) ;
#12556 = EDGE_CURVE ( 'NONE', #22403, #3079, #7516, .T. ) ;
#12557 = COORDINATED_UNIVERSAL_TIME_OFFSET ( 0, 0, .AHEAD. ) ;
#12558 = CYLINDRICAL_SURFACE ( 'NONE', #20936, 2.500000000000000444 ) ;
#12559 = ORIENTED_EDGE ( 'NONE', *, *, #11608, .T. ) ;
#12560 = LOCAL_TIME ( 14, 11, 27.00000000000000000, #20919 ) ;
#12561 = CARTESIAN_POINT ( 'NONE',  ( 84.26187758838335640, -12.29469986460233599, 13.00000000000000000 ) ) ;
#12562 = APPROVAL_PERSON_ORGANIZATION ( #8644, #16473, #6500 ) ;
#12563 = COORDINATED_UNIVERSAL_TIME_OFFSET ( 0, 0, .AHEAD. ) ;
#12564 = CONICAL_SURFACE ( 'NONE', #8820, 2.729132938682640397, 1.047197551196598297 ) ;
#12565 = CC_DESIGN_SECURITY_CLASSIFICATION ( #22778, ( #23508 ) ) ;
#12566 = APPROVAL_ROLE ( '' ) ;
#12567 = DIRECTION ( 'NONE',  ( -3.210834492181045054E-17, 2.441916418604790135E-15, 1.000000000000000000 ) ) ;
#12568 = CARTESIAN_POINT ( 'NONE',  ( 33.37436288052550992, -3.059220458576291435, 10.50000000000019895 ) ) ;
#12569 = ORIENTED_EDGE ( 'NONE', *, *, #5584, .T. ) ;
#12570 = CARTESIAN_POINT ( 'NONE',  ( -12.33340651292470014, 21.13490689743859718, -3.289309883929029635E-15 ) ) ;
#12571 = EDGE_CURVE ( 'NONE', #20636, #12251, #8266, .T. ) ;
#12572 = SECURITY_CLASSIFICATION ( '', '', #6530 ) ;
#12573 = ORIENTED_EDGE ( 'NONE', *, *, #6785, .F. ) ;
#12574 = CC_DESIGN_APPROVAL ( #20903, ( #4225 ) ) ;
#12575 = CARTESIAN_POINT ( 'NONE',  ( 36.50043006307940630, 22.92019839501219991, 12.99999999999979927 ) ) ;
#12576 = CARTESIAN_POINT ( 'NONE',  ( 114.3964932440919995, -22.26358663789240211, -13.00000000000000000 ) ) ;
#12577 = LINE ( 'NONE', #10688, #2917 ) ;
#12578 = ORIENTED_EDGE ( 'NONE', *, *, #15181, .T. ) ;
#12579 = APPROVAL ( #18848, 'UNSPECIFIED' ) ;
#12580 = PRODUCT_RELATED_PRODUCT_CATEGORY ( 'detail', '', ( #7215 ) ) ;
#12581 = FACE_BOUND ( 'NONE', #16327, .T. ) ;
#12582 = CYLINDRICAL_SURFACE ( 'NONE', #862, 5.999999999999998224 ) ;
#12583 = ORIENTED_EDGE ( 'NONE', *, *, #644, .T. ) ;
#12584 = CC_DESIGN_SECURITY_CLASSIFICATION ( #22797, ( #23495 ) ) ;
#12585 = ORIENTED_EDGE ( 'NONE', *, *, #817, .T. ) ;
#12586 = EDGE_CURVE ( 'NONE', #5941, #11278, #20391, .T. ) ;
#12587 = ADVANCED_FACE ( 'NONE', ( #11951 ), #1030, .F. ) ;
#12588 = PERSON_AND_ORGANIZATION ( #11966, #8758 ) ;
#12589 = EDGE_LOOP ( 'NONE', ( #7434, #8194, #10714, #19579 ) ) ;
#12590 = EDGE_LOOP ( 'NONE', ( #21269, #15414, #1840, #22755, #11424 ) ) ;
#12591 = CC_DESIGN_PERSON_AND_ORGANIZATION_ASSIGNMENT ( #7870, #14988, ( #14812 ) ) ;
#12592 = DIRECTION ( 'NONE',  ( 0.000000000000000000, 0.000000000000000000, -1.000000000000000000 ) ) ;
#12593 = APPROVAL_ROLE ( '' ) ;
#12594 = CC_DESIGN_SECURITY_CLASSIFICATION ( #6898, ( #19398 ) ) ;
#12595 = DIRECTION ( 'NONE',  ( 0.9730401042858021210, -0.2306359803922085061, 0.000000000000000000 ) ) ;
#12596 = ITEM_DEFINED_TRANSFORMATION ( 'NONE', 'NONE', #4192,  #12739 ) ;
#12597 = PLANE ( 'NONE',  #15752 ) ;
#12598 = VECTOR ( 'NONE', #7485, 1000.000000000000000 ) ;
#12599 = SECURITY_CLASSIFICATION ( '', '', #13496 ) ;
#12600 = CARTESIAN_POINT ( 'NONE',  ( 43.84419854219520829, 9.774809681453278998, -65.86501949894326913 ) ) ;
#12601 = PERSON_AND_ORGANIZATION_ROLE ( 'creator' ) ;
#12602 = ADVANCED_FACE ( 'NONE', ( #23061 ), #14340, .T. ) ;
#12603 = EDGE_LOOP ( 'NONE', ( #2166, #6119, #2513, #13328, #10058 ) ) ;
#12604 = CYLINDRICAL_SURFACE ( 'NONE', #10289, 3.499999999999999556 ) ;
#12605 = CARTESIAN_POINT ( 'NONE',  ( 35.88249351768550355, 10.99110981181069846, 10.50000000000020073 ) ) ;
#12606 = VERTEX_POINT ( 'NONE', #3002 ) ;
#12607 = CC_DESIGN_APPROVAL ( #9224, ( #14859 ) ) ;
#12608 = DIRECTION ( 'NONE',  ( -6.193954341422139021E-17, -4.965628413872130537E-15, -1.000000000000000000 ) ) ;
#12609 = DIRECTION ( 'NONE',  ( -1.751019220569994795E-16, -2.300154215587015208E-15, -1.000000000000000000 ) ) ;
#12610 = DIRECTION ( 'NONE',  ( -0.7071067811865475727, 0.000000000000000000, -0.7071067811865475727 ) ) ;
#12611 = ORIENTED_EDGE ( 'NONE', *, *, #10690, .T. ) ;
#12612 = EDGE_LOOP ( 'NONE', ( #21694, #19163 ) ) ;
#12613 = CARTESIAN_POINT ( 'NONE',  ( -26.68810977484059777, -6.639828994528089723, 2.501000000000090484 ) ) ;
#12614 = AXIS2_PLACEMENT_3D ( 'NONE', #4558, #20163, #11389 ) ;
#12615 = VERTEX_POINT ( 'NONE', #22947 ) ;
#12616 = EDGE_CURVE ( 'NONE', #8149, #8186, #23412, .T. ) ;
#12617 = CALENDAR_DATE ( 2026, 31, 10 ) ;
#12619 = ADVANCED_FACE ( 'NONE', ( #20820 ), #8133, .T. ) ;
#12618 = ORIENTED_EDGE ( 'NONE', *, *, #4970, .F. ) ;
#12620 = ORIENTED_EDGE ( 'NONE', *, *, #18231, .T. ) ;
#12621 = DIRECTION ( 'NONE',  ( 0.9730401042858035643, -0.2306359803922028717, -5.959266323858667582E-17 ) ) ;
#12622 = CIRCLE ( 'NONE', #17549, 2.500000000000000000 ) ;
#12623 = PLANE ( 'NONE',  #18354 ) ;
#12624 = CC_DESIGN_APPROVAL ( #11838, ( #10735 ) ) ;
#12625 = DIRECTION ( 'NONE',  ( 0.9730401042858035643, -0.2306359803922031215, -4.456532139458528310E-16 ) ) ;
#12626 = DATE_AND_TIME ( #7396, #3118 ) ;
#12627 = DIRECTION ( 'NONE',  ( 4.027614241767943373E-31, 2.300154215587010080E-15, 1.000000000000000000 ) ) ;
#12628 = VECTOR ( 'NONE', #15704, 1000.000000000000000 ) ;
#12629 = PLANE ( 'NONE',  #1902 ) ;
#12630 = CC_DESIGN_APPROVAL ( #1243, ( #1530 ) ) ;
#12631 = DIRECTION ( 'NONE',  ( 1.000000000000000000, 0.000000000000000000, 0.000000000000000000 ) ) ;
#12632 = AXIS2_PLACEMENT_3D ( 'NONE', #18175, #12492, #12610 ) ;
#12633 = DIRECTION ( 'NONE',  ( 0.000000000000000000, -5.060555282020610014E-15, -1.000000000000000000 ) ) ;
#12634 = PERSON_AND_ORGANIZATION_ROLE ( 'creator' ) ;
#12635 = VECTOR ( 'NONE', #8261, 1000.000000000000000 ) ;
#12636 = CARTESIAN_POINT ( 'NONE',  ( -65.86009907636304206, -2.344873239356385142, -5.892192847027045428E-15 ) ) ;
#12637 = FACE_OUTER_BOUND ( 'NONE', #7262, .T. ) ;
#12638 =( REPRESENTATION_RELATIONSHIP ('NONE','NONE', #19303, #12659 ) REPRESENTATION_RELATIONSHIP_WITH_TRANSFORMATION ( #11733 )SHAPE_REPRESENTATION_RELATIONSHIP( ) );
#12639 = VECTOR ( 'NONE', #19181, 1000.000000000000000 ) ;
#12640 = CARTESIAN_POINT ( 'NONE',  ( -23.50000000000000000, -19.99999999999999289, 2.500000000000000000 ) ) ;
#12641 = DIRECTION ( 'NONE',  ( -5.964507377817318600E-17, -4.861311874385510251E-15, -1.000000000000000000 ) ) ;
#12642 = ADVANCED_FACE ( 'NONE', ( #6337 ), #16996, .T. ) ;
#12643 = CARTESIAN_POINT ( 'NONE',  ( 36.68971944905818816, 14.39675017681109992, 26.49999999999997513 ) ) ;
#12644 = VERTEX_POINT ( 'NONE', #22830 ) ;
#12645 = AXIS2_PLACEMENT_3D ( 'NONE', #8519, #19424, #13961 ) ;
#12646 = CYLINDRICAL_SURFACE ( 'NONE', #11505, 2.066999999999999726 ) ;
#12647 = EDGE_CURVE ( 'NONE', #9648, #3048, #20934, .T. ) ;
#12648 = APPROVAL_PERSON_ORGANIZATION ( #17169, #21986, #19420 ) ;
#12649 = ORIENTED_EDGE ( 'NONE', *, *, #9853, .T. ) ;
#12650 = DIRECTION ( 'NONE',  ( -0.04564792618501069266, -0.9989575901083128651, 2.775557561562892534E-15 ) ) ;
#12651 = DIRECTION ( 'NONE',  ( 6.123230174520370177E-17, 4.962644601432260272E-15, 1.000000000000000000 ) ) ;
#12652 = VERTEX_POINT ( 'NONE', #978 ) ;
#12653 = AXIS2_PLACEMENT_3D ( 'NONE', #19344, #21231, #20889 ) ;
#12654 = CONICAL_SURFACE ( 'NONE', #10393, 2.283500000000000529, 0.7853981633974539411 ) ;
#12655 = FACE_BOUND ( 'NONE', #5118, .T. ) ;
#12656 = ORIENTED_EDGE ( 'NONE', *, *, #20098, .T. ) ;
#12657 = CIRCLE ( 'NONE', #5432, 3.500000000000000444 ) ;
#12658 = DIRECTION ( 'NONE',  ( 0.2306359803922076457, 0.9730401042858025651, 0.000000000000000000 ) ) ;
#12659 = SHAPE_REPRESENTATION ( '1602p_c_10', ( #12739 ), #3270 ) ;
#12660 = DATE_TIME_ROLE ( 'creation_date' ) ;
#12661 = CARTESIAN_POINT ( 'NONE',  ( -0.5391976746782148888, 18.33937061236850141, 3.301631463538509622E-17 ) ) ;
#12662 = LINE ( 'NONE', #12876, #16816 ) ;
#12663 = DIRECTION ( 'NONE',  ( -0.9997651245102161521, -0.02167246670483386276, 0.000000000000000000 ) ) ;
#12664 = CARTESIAN_POINT ( 'NONE',  ( 0.000000000000000000, 0.000000000000000000, 0.000000000000000000 ) ) ;
#12665 = EDGE_CURVE ( 'NONE', #2629, #17907, #19938, .T. ) ;
#12666 = AXIS2_PLACEMENT_3D ( 'NONE', #21808, #12906, #20279 ) ;
#12667 = CARTESIAN_POINT ( 'NONE',  ( -20.00000000000000000, -20.00000000000000000, 2.500000000000000000 ) ) ;
#12668 = LINE ( 'NONE', #3624, #18897 ) ;
#12669 = DIRECTION ( 'NONE',  ( 0.2306359803922080898, 0.9730401042858024541, -2.572202231434325988E-16 ) ) ;
#12670 = PLANE ( 'NONE',  #6111 ) ;
#12671 = ORIENTED_EDGE ( 'NONE', *, *, #11041, .F. ) ;
#12672 = PLANE ( 'NONE',  #10783 ) ;
#12673 = CYLINDRICAL_SURFACE ( 'NONE', #5769, 5.999999999999999112 ) ;
#12674 = EDGE_LOOP ( 'NONE', ( #22285, #3276, #2867, #9620, #17028 ) ) ;
#12675 = CARTESIAN_POINT ( 'NONE',  ( 37.10730959030829723, 23.96304573415820016, 11.00000000000000000 ) ) ;
#12676 = CARTESIAN_POINT ( 'NONE',  ( 1.358598381910800010E-16, -1.434096706618689895E-15, 8.874009851233079243E-14 ) ) ;
#12677 = ORIENTED_EDGE ( 'NONE', *, *, #8399, .T. ) ;
#12678 = CALENDAR_DATE ( 2026, 31, 10 ) ;
#12679 = FACE_BOUND ( 'NONE', #10000, .T. ) ;
#12680 = AXIS2_PLACEMENT_3D ( 'NONE', #14309, #9082, #12772 ) ;
#12681 = VERTEX_POINT ( 'NONE', #17391 ) ;
#12682 = CARTESIAN_POINT ( 'NONE',  ( 5.000000000000000000, -29.85000000000000142, 12.00000000000000000 ) ) ;
#12683 = COORDINATED_UNIVERSAL_TIME_OFFSET ( 0, 0, .AHEAD. ) ;
#12684 = AXIS2_PLACEMENT_3D ( 'NONE', #694, #15190, #22659 ) ;
#12685 = EDGE_CURVE ( 'NONE', #15635, #813, #12475, .T. ) ;
#12686 = ADVANCED_FACE ( 'NONE', ( #11821 ), #19281, .F. ) ;
#12687 = DATE_TIME_ROLE ( 'classification_date' ) ;
#12688 = CARTESIAN_POINT ( 'NONE',  ( -55.91259579215963527, 7.707349321388969443, 7.199999999999994849 ) ) ;
#12689 = DIRECTION ( 'NONE',  ( 0.2306359803922028995, 0.9730401042858036753, -9.756037151021835575E-16 ) ) ;
#12690 = VERTEX_POINT ( 'NONE', #4682 ) ;
#12691 = CARTESIAN_POINT ( 'NONE',  ( -32.65691263631629226, 9.274125246214079965, 5.000000000000000000 ) ) ;
#12692 = EDGE_CURVE ( 'NONE', #6798, #6743, #23431, .T. ) ;
#12693 = EDGE_CURVE ( 'NONE', #1981, #22224, #298, .T. ) ;
#12694 = ORIENTED_EDGE ( 'NONE', *, *, #4112, .T. ) ;
#12695 = FACE_OUTER_BOUND ( 'NONE', #1976, .T. ) ;
#12696 = DIRECTION ( 'NONE',  ( -0.2306359803922028995, -0.9730401042858035643, 3.648592655857288816E-32 ) ) ;
#12697 = DIRECTION ( 'NONE',  ( 0.1630842657209342073, 0.6880432561069562691, 0.7071067811865482389 ) ) ;
#12698 = VERTEX_POINT ( 'NONE', #10272 ) ;
#12699 = DIRECTION ( 'NONE',  ( 0.000000000000000000, 1.734723475976806848E-16, 1.000000000000000000 ) ) ;
#12700 = CARTESIAN_POINT ( 'NONE',  ( 39.94748832170340336, 24.67242251356961091, 13.00000000000000000 ) ) ;
#12701 = ORIENTED_EDGE ( 'NONE', *, *, #657, .F. ) ;
#12702 = APPLICATION_PROTOCOL_DEFINITION ( 'international standard', 'config_control_design', 1994, #14734 ) ;
#12703 = VERTEX_POINT ( 'NONE', #21169 ) ;
#12704 = VERTEX_POINT ( 'NONE', #13474 ) ;
#12705 = CYLINDRICAL_SURFACE ( 'NONE', #22473, 3.499999999999999556 ) ;
#12706 = PERSON_AND_ORGANIZATION ( #11966, #8758 ) ;
#12707 = ADVANCED_FACE ( 'NONE', ( #15832 ), #3351, .T. ) ;
#12708 = DIRECTION ( 'NONE',  ( -0.2306359803922033158, -0.9730401042858034533, 0.000000000000000000 ) ) ;
#12709 = PERSON_AND_ORGANIZATION_ROLE ( 'classification_officer' ) ;
#12710 = CYLINDRICAL_SURFACE ( 'NONE', #7784, 0.4000000000000010214 ) ;
#12711 = TOROIDAL_SURFACE ( 'NONE', #8548, 2.600000000000000089, 0.1000000000000000056 ) ;
#12712 = CC_DESIGN_DATE_AND_TIME_ASSIGNMENT ( #3321, #11704, ( #3753 ) ) ;
#12713 = APPROVAL ( #1904, 'UNSPECIFIED' ) ;
#12714 = FACE_BOUND ( 'NONE', #9169, .T. ) ;
#12715 = ADVANCED_FACE ( 'NONE', ( #12057 ), #19283, .F. ) ;
#12716 = EDGE_CURVE ( 'NONE', #11260, #7299, #12172, .T. ) ;
#12717 = SHAPE_DEFINITION_REPRESENTATION ( #6642, #1107 ) ;
#12718 = PRODUCT ( '1602p_c_44', '1602p_c_44', '', ( #486 ) ) ;
#12719 = EDGE_LOOP ( 'NONE', ( #698, #1517, #7128, #10168 ) ) ;
#12720 = DIRECTION ( 'NONE',  ( -0.9730401042858036753, 0.2306359803922028995, 5.959266323858677443E-17 ) ) ;
#12721 = VERTEX_POINT ( 'NONE', #19872 ) ;
#12722 = CARTESIAN_POINT ( 'NONE',  ( -62.73971250800079957, -25.32895006819559924, 5.000000000000000000 ) ) ;
#12723 = VECTOR ( 'NONE', #13873, 999.9999999999998863 ) ;
#12724 = CARTESIAN_POINT ( 'NONE',  ( 5.000000000000000000, -28.60000000000000142, 2.500000000000000000 ) ) ;
#12725 = DIRECTION ( 'NONE',  ( 0.000000000000000000, 0.000000000000000000, -1.000000000000000000 ) ) ;
#12726 = VERTEX_POINT ( 'NONE', #14172 ) ;
#12727 = VERTEX_POINT ( 'NONE', #23173 ) ;
#12728 = CARTESIAN_POINT ( 'NONE',  ( -20.00000000000000000, -25.00000000000000000, 5.500000000004569678 ) ) ;
#12729 = ORIENTED_EDGE ( 'NONE', *, *, #20787, .F. ) ;
#12730 = CALENDAR_DATE ( 2026, 31, 10 ) ;
#12731 = ORIENTED_EDGE ( 'NONE', *, *, #10616, .T. ) ;
#12732 = ORIENTED_EDGE ( 'NONE', *, *, #4050, .F. ) ;
#12733 = CARTESIAN_POINT ( 'NONE',  ( -55.91259579215963527, 7.707349321388969443, 7.200000000000000178 ) ) ;
#12734 = CARTESIAN_POINT ( 'NONE',  ( 31.49315201223960159, -2.613324229818170252, -14.15470053837965025 ) ) ;
#12735 = PERSON_AND_ORGANIZATION ( #11966, #8758 ) ;
#12736 = DIRECTION ( 'NONE',  ( 9.055045682909269434E-14, 0.000000000000000000, -1.000000000000000000 ) ) ;
#12737 = ADVANCED_FACE ( 'NONE', ( #9170 ), #17849, .T. ) ;
#12738 = CARTESIAN_POINT ( 'NONE',  ( -26.75617730459320143, 6.359992804688110901, -2.500999999999729884 ) ) ;
#12739 = AXIS2_PLACEMENT_3D ( 'NONE', #2569, #13380, #415 ) ;
#12740 = EDGE_CURVE ( 'NONE', #22303, #13648, #5251, .T. ) ;
#12741 = EDGE_CURVE ( 'NONE', #3857, #503, #11335, .T. ) ;
#12742 = ORIENTED_EDGE ( 'NONE', *, *, #10986, .F. ) ;
#12743 = AXIS2_PLACEMENT_3D ( 'NONE', #21134, #6670, #3432 ) ;
#12744 = CARTESIAN_POINT ( 'NONE',  ( 37.27955344062029752, 9.375336445360789028, 29.25000000000000000 ) ) ;
#12745 = SECURITY_CLASSIFICATION_LEVEL ( 'unclassified' ) ;
#12746 = LINE ( 'NONE', #14636, #19357 ) ;
#12747 = DIRECTION ( 'NONE',  ( -3.210834492194360164E-17, 2.441916418604790135E-15, 1.000000000000000000 ) ) ;
#12748 = DIRECTION ( 'NONE',  ( 0.000000000000000000, -2.891431443143872083E-16, 1.000000000000000000 ) ) ;
#12749 = CARTESIAN_POINT ( 'NONE',  ( 62.70840910389689782, 3.348031886875269869, 1.061114750357439988E-14 ) ) ;
#12750 = FACE_OUTER_BOUND ( 'NONE', #8231, .T. ) ;
#12751 = ORIENTED_EDGE ( 'NONE', *, *, #675, .F. ) ;
#12752 = CARTESIAN_POINT ( 'NONE',  ( 33.61053995400052941, 9.178437802375466248, 8.940674882554530356 ) ) ;
#12753 = UNCERTAINTY_MEASURE_WITH_UNIT (LENGTH_MEASURE( 1.000000000000000082E-05 ), #19172, 'distance_accuracy_value', 'NONE');
#12754 = ORIENTED_EDGE ( 'NONE', *, *, #32, .T. ) ;
#12755 = CARTESIAN_POINT ( 'NONE',  ( -27.39127619791450030, 6.327883175579949615, -5.000000000000000000 ) ) ;
#12756 = CARTESIAN_POINT ( 'NONE',  ( 58.73439644601039333, 17.65016624305030035, 11.75000000000000000 ) ) ;
#12757 = ORIENTED_EDGE ( 'NONE', *, *, #18960, .T. ) ;
#12758 = CYLINDRICAL_SURFACE ( 'NONE', #14910, 1.749999999999997780 ) ;
#12760 = ORIENTED_EDGE ( 'NONE', *, *, #4250, .T. ) ;
#12759 = EDGE_CURVE ( 'NONE', #4396, #18309, #6782, .T. ) ;
#12761 = DIRECTION ( 'NONE',  ( 0.005235963827110211646, -0.9999862922474493931, -5.936218956700079549E-19 ) ) ;
#12762 = APPROVAL_STATUS ( 'not_yet_approved' ) ;
#12763 = CARTESIAN_POINT ( 'NONE',  ( -30.72370968135370006, -6.660959539311599897, 2.999707106781279720 ) ) ;
#12764 = EDGE_CURVE ( 'NONE', #19959, #8630, #19626, .T. ) ;
#12765 =( REPRESENTATION_RELATIONSHIP ('NONE','NONE', #18771, #6895 ) REPRESENTATION_RELATIONSHIP_WITH_TRANSFORMATION ( #10996 )SHAPE_REPRESENTATION_RELATIONSHIP( ) );
#12766 = DIRECTION ( 'NONE',  ( 0.005235963827110211646, -0.9999862922474493931, -5.936218956700079549E-19 ) ) ;
#12767 = EDGE_CURVE ( 'NONE', #14140, #11059, #20792, .T. ) ;
#12768 = DIRECTION ( 'NONE',  ( -0.9730401042858036753, 0.2306359803922028995, 5.959266323858677443E-17 ) ) ;
#12769 = DIRECTION ( 'NONE',  ( 1.000000000000000000, 0.000000000000000000, 0.000000000000000000 ) ) ;
#12770 = EDGE_CURVE ( 'NONE', #19953, #7688, #3471, .T. ) ;
#12771 = AXIS2_PLACEMENT_3D ( 'NONE', #17152, #9568, #524 ) ;
#12772 = DIRECTION ( 'NONE',  ( 1.000000000000000000, -2.611676738638919574E-15, 0.000000000000000000 ) ) ;
#12773 = CARTESIAN_POINT ( 'NONE',  ( 36.57467860885130051, 21.71590586959130320, -11.00000000000049916 ) ) ;
#12774 = CARTESIAN_POINT ( 'NONE',  ( -29.01760921662840076, 6.974057232812999274, -5.000000000000000000 ) ) ;
#12775 = DESIGN_CONTEXT ( 'detailed design', #13979, 'design' ) ;
#12776 = CARTESIAN_POINT ( 'NONE',  ( 36.89121352362743522, 22.27682603178732279, -15.00000000000051514 ) ) ;
#12777 = FACE_OUTER_BOUND ( 'NONE', #18607, .T. ) ;
#12778 = DIRECTION ( 'NONE',  ( -0.005235964026270697493, 0.9999862922464064496, 1.340741286434373073E-35 ) ) ;
#12779 = ORIENTED_EDGE ( 'NONE', *, *, #20948, .F. ) ;
#12780 = ADVANCED_BREP_SHAPE_REPRESENTATION ( '', ( #1349, #12739 ), #21837 ) ;
#12781 = ORIENTED_EDGE ( 'NONE', *, *, #7249, .T. ) ;
#12782 = DIRECTION ( 'NONE',  ( -1.000000000000000000, 2.275047181608927151E-16, 0.000000000000000000 ) ) ;
#12783 = FACE_OUTER_BOUND ( 'NONE', #16173, .T. ) ;
#12784 = ORIENTED_EDGE ( 'NONE', *, *, #12356, .F. ) ;
#12785 = PLANE ( 'NONE',  #7325 ) ;
#12786 = ORIENTED_EDGE ( 'NONE', *, *, #9877, .T. ) ;
#12787 = AXIS2_PLACEMENT_3D ( 'NONE', #5774, #9460, #20621 ) ;
#12788 = VECTOR ( 'NONE', #6652, 1000.000000000000114 ) ;
#12789 = LINE ( 'NONE', #3400, #22284 ) ;
#12790 = AXIS2_PLACEMENT_3D ( 'NONE', #17275, #13703, #12299 ) ;
#12791 = APPROVAL_ROLE ( '' ) ;
#12792 = APPROVAL ( #18934, 'UNSPECIFIED' ) ;
#12793 = DATE_AND_TIME ( #20149, #4608 ) ;
#12794 = DIRECTION ( 'NONE',  ( -0.9999862922474492821, -0.005235963827121951387, 1.187304881134294758E-16 ) ) ;
#12795 = AXIS2_PLACEMENT_3D ( 'NONE', #5609, #23304, #7521 ) ;
#12796 = DIRECTION ( 'NONE',  ( -0.6660003063074659835, 0.7459514675891198987, 0.000000000000000000 ) ) ;
#12797 = VERTEX_POINT ( 'NONE', #15940 ) ;
#12798 = AXIS2_PLACEMENT_3D ( 'NONE', #14687, #5543, #20035 ) ;
#12799 = VECTOR ( 'NONE', #23322, 1000.000000000000000 ) ;
#12800 = VECTOR ( 'NONE', #3098, 1000.000000000000000 ) ;
#12801 = ORIENTED_EDGE ( 'NONE', *, *, #6417, .T. ) ;
#12802 = DIRECTION ( 'NONE',  ( 0.9949874374308235181, 0.09999999677421517186, -1.144917494144692682E-14 ) ) ;
#12803 = FACE_OUTER_BOUND ( 'NONE', #9599, .T. ) ;
#12804 = CARTESIAN_POINT ( 'NONE',  ( 35.59419854219520118, 9.774809681453319854, -19.78350000000000009 ) ) ;
#12805 = EDGE_LOOP ( 'NONE', ( #6570, #881, #1543, #16263 ) ) ;
#12806 = ADVANCED_FACE ( 'NONE', ( #18082 ), #10746, .T. ) ;
#12807 = CALENDAR_DATE ( 2026, 31, 10 ) ;
#12808 = FACE_OUTER_BOUND ( 'NONE', #1250, .T. ) ;
#12809 = VERTEX_POINT ( 'NONE', #8 ) ;
#12810 = APPROVAL_ROLE ( '' ) ;
#12811 = VERTEX_POINT ( 'NONE', #8710 ) ;
#12812 = ORIENTED_EDGE ( 'NONE', *, *, #22952, .T. ) ;
#12813 = CARTESIAN_POINT ( 'NONE',  ( -26.00000000000179767, -20.00000000055539928, -6.749999999994109601 ) ) ;
#12814 = AXIS2_PLACEMENT_3D ( 'NONE', #1068, #15570, #21039 ) ;
#12815 = DATE_AND_TIME ( #21710, #12263 ) ;
#12816 = CIRCLE ( 'NONE', #7132, 2.500000000000000444 ) ;
#12817 = FACE_OUTER_BOUND ( 'NONE', #11161, .T. ) ;
#12818 = PERSON_AND_ORGANIZATION ( #4287, #13260 ) ;
#12819 = AXIS2_PLACEMENT_3D ( 'NONE', #18587, #15244, #16542 ) ;
#12820 = FACE_OUTER_BOUND ( 'NONE', #7269, .T. ) ;
#12821 = CARTESIAN_POINT ( 'NONE',  ( -26.72214353971689960, -0.1399180949200569957, -2.500999999999910184 ) ) ;
#12822 = CIRCLE ( 'NONE', #4090, 2.500000000000000000 ) ;
#12823 = APPROVAL_DATE_TIME ( #18530, #17515 ) ;
#12824 = VERTEX_POINT ( 'NONE', #7167 ) ;
#12825 = AXIS2_PLACEMENT_3D ( 'NONE', #9717, #6130, #11734 ) ;
#12826 = FACE_OUTER_BOUND ( 'NONE', #2212, .T. ) ;
#12827 = ORIENTED_EDGE ( 'NONE', *, *, #8370, .T. ) ;
#12828 = ADVANCED_FACE ( 'NONE', ( #9055 ), #16287, .T. ) ;
#12829 = FACE_OUTER_BOUND ( 'NONE', #4629, .T. ) ;
#12830 = DIRECTION ( 'NONE',  ( 2.086281924601080239E-16, 1.946516371809877606E-18, -1.000000000000000000 ) ) ;
#12831 = DIRECTION ( 'NONE',  ( 0.7071067811865476838, -1.387778780781444689E-15, 0.7071067811865473507 ) ) ;
#12832 = VERTEX_POINT ( 'NONE', #12294 ) ;
#12833 = EDGE_LOOP ( 'NONE', ( #19322, #4018, #17200, #5474 ) ) ;
#12834 = CARTESIAN_POINT ( 'NONE',  ( -22.52506282043179908, 26.45208917575140006, -5.499999999994999555 ) ) ;
#12835 = ORIENTED_EDGE ( 'NONE', *, *, #10518, .F. ) ;
#12836 = APPROVAL ( #15285, 'UNKNOWN' ) ;
#12837 = MECHANICAL_CONTEXT ( 'NONE', #15501, 'mechanical' ) ;
#12838 = ORIENTED_EDGE ( 'NONE', *, *, #12556, .F. ) ;
#12839 = ORIENTED_EDGE ( 'NONE', *, *, #3622, .T. ) ;
#12840 = CARTESIAN_POINT ( 'NONE',  ( -20.18494928784681264, 20.45893982632658492, -4.999999999995553779 ) ) ;
#12841 = FACE_OUTER_BOUND ( 'NONE', #5668, .T. ) ;
#12842 = DATE_AND_TIME ( #13088, #7300 ) ;
#12843 = EDGE_CURVE ( 'NONE', #13304, #23125, #8836, .T. ) ;
#12844 = DIRECTION ( 'NONE',  ( -0.2306359803922080898, -0.9730401042858024541, 2.572202231434325988E-16 ) ) ;
#12845 = EDGE_CURVE ( 'NONE', #8909, #5287, #21627, .T. ) ;
#12846 = LINE ( 'NONE', #20323, #11033 ) ;
#12847 = ORIENTED_EDGE ( 'NONE', *, *, #5076, .F. ) ;
#12848 = DIRECTION ( 'NONE',  ( -6.123230199561459225E-17, -4.868008300101910084E-15, -1.000000000000000000 ) ) ;
#12849 = PERSON_AND_ORGANIZATION_ROLE ( 'classification_officer' ) ;
#12850 = VERTEX_POINT ( 'NONE', #16069 ) ;
#12851 = LINE ( 'NONE', #3814, #16672 ) ;
#12852 = CYLINDRICAL_SURFACE ( 'NONE', #12404, 1.250000000000000222 ) ;
#12853 = LINE ( 'NONE', #8949, #7085 ) ;
#12854 = ADVANCED_FACE ( 'NONE', ( #14049 ), #14521, .F. ) ;
#12855 = DIRECTION ( 'NONE',  ( 0.2306359803922083396, 0.9730401042858023430, 1.301042606982605826E-13 ) ) ;
#12856 = CARTESIAN_POINT ( 'NONE',  ( -26.68810977484059777, -6.639828994528159889, 2.500000000000090150 ) ) ;
#12857 = EDGE_LOOP ( 'NONE', ( #18012, #14834, #4036, #19664, #10001 ) ) ;
#12858 = DIRECTION ( 'NONE',  ( -0.2306359803922087282, -0.9730401042858021210, 5.204170427930421283E-15 ) ) ;
#12859 = APPROVAL ( #3317, 'UNSPECIFIED' ) ;
#12860 = ORIENTED_EDGE ( 'NONE', *, *, #12198, .F. ) ;
#12861 = CC_DESIGN_DATE_AND_TIME_ASSIGNMENT ( #22786, #1405, ( #13884 ) ) ;
#12862 = VERTEX_POINT ( 'NONE', #21757 ) ;
#12863 = DIRECTION ( 'NONE',  ( -7.008869410147150310E-16, 5.150359455772420684E-15, 1.000000000000000000 ) ) ;
#12864 = CARTESIAN_POINT ( 'NONE',  ( 0.000000000000000000, 2.499999999999998224, 5.000000000000000000 ) ) ;
#12865 = ORIENTED_EDGE ( 'NONE', *, *, #1703, .T. ) ;
#12866 = EDGE_CURVE ( 'NONE', #1999, #16389, #16175, .T. ) ;
#12867 = FACE_OUTER_BOUND ( 'NONE', #19977, .T. ) ;
#12868 = EDGE_CURVE ( 'NONE', #22213, #4561, #17739, .T. ) ;
#12869 = ORIENTED_EDGE ( 'NONE', *, *, #22715, .T. ) ;
#12870 = CC_DESIGN_PERSON_AND_ORGANIZATION_ASSIGNMENT ( #8222, #963, ( #1527 ) ) ;
#12871 = LINE ( 'NONE', #10993, #21510 ) ;
#12872 = LOCAL_TIME ( 14, 11, 27.00000000000000000, #16284 ) ;
#12873 = COORDINATED_UNIVERSAL_TIME_OFFSET ( 0, 0, .AHEAD. ) ;
#12874 = AXIS2_PLACEMENT_3D ( 'NONE', #10383, #6438, #3344 ) ;
#12875 = FACE_OUTER_BOUND ( 'NONE', #15321, .T. ) ;
#12876 = CARTESIAN_POINT ( 'NONE',  ( -26.68881687192900287, -6.639832696913689603, 2.500292893218909906 ) ) ;
#12877 = LINE ( 'NONE', #5517, #16986 ) ;
#12878 =( NAMED_UNIT ( * ) PLANE_ANGLE_UNIT ( ) SI_UNIT ( $, .RADIAN. ) );
#12879 = DIRECTION ( 'NONE',  ( -0.4188265566777199522, -0.9080662505684728991, 2.203974058899820124E-15 ) ) ;
#12880 = DIRECTION ( 'NONE',  ( 1.000000000000000000, 9.250447630115842075E-11, -1.110223024625156383E-14 ) ) ;
#12881 = CARTESIAN_POINT ( 'NONE',  ( -62.91228861290962726, 7.630356943151853422, 4.999999999999999112 ) ) ;
#12882 = ADVANCED_FACE ( 'NONE', ( #6815 ), #21289, .F. ) ;
#12883 = CARTESIAN_POINT ( 'NONE',  ( 36.78282996199610722, 11.03463321983590006, 27.68999999999999773 ) ) ;
#12884 = DIRECTION ( 'NONE',  ( -0.07397971354964476276, -0.9972597464969256142, 2.428612866367529538E-15 ) ) ;
#12885 = CIRCLE ( 'NONE', #22365, 4.999999999999997335 ) ;
#12886 = CARTESIAN_POINT ( 'NONE',  ( 6.500000000000000000, -17.30000000000000071, 5.000000000000000000 ) ) ;
#12887 = ORIENTED_EDGE ( 'NONE', *, *, #2605, .T. ) ;
#12888 = EDGE_CURVE ( 'NONE', #14815, #8021, #11449, .T. ) ;
#12889 = ORIENTED_EDGE ( 'NONE', *, *, #3065, .F. ) ;
#12890 = CARTESIAN_POINT ( 'NONE',  ( 113.4570673249340018, -28.10438863268850085, -2.700000000000000178 ) ) ;
#12891 = CARTESIAN_POINT ( 'NONE',  ( 37.46113131852679601, -4.027891576221680481, -13.00000000000000000 ) ) ;
#12892 = AXIS2_PLACEMENT_3D ( 'NONE', #2550, #8017, #20714 ) ;
#12893 = EDGE_LOOP ( 'NONE', ( #13139, #19700 ) ) ;
#12894 = EDGE_CURVE ( 'NONE', #2368, #3573, #9433, .T. ) ;
#12895 = CARTESIAN_POINT ( 'NONE',  ( -26.26776695296636888, -28.59999999999999787, 20.76776695296636888 ) ) ;
#12896 = EDGE_LOOP ( 'NONE', ( #606, #13489, #2192, #23070, #15731 ) ) ;
#12897 = EDGE_CURVE ( 'NONE', #11373, #12726, #16516, .T. ) ;
#12898 = CARTESIAN_POINT ( 'NONE',  ( 58.49563186522070168, 17.70675969991879839, -13.00000000000049916 ) ) ;
#12899 = CALENDAR_DATE ( 2026, 31, 10 ) ;
#12900 = CARTESIAN_POINT ( 'NONE',  ( 36.20426423164212792, 11.75447824097759231, -8.759424124907058129 ) ) ;
#12901 = PRODUCT_DEFINITION_SHAPE ( 'NONE', 'NONE',  #23498 ) ;
#12902 = CC_DESIGN_APPROVAL ( #17811, ( #16680 ) ) ;
#12903 = COORDINATED_UNIVERSAL_TIME_OFFSET ( 0, 0, .AHEAD. ) ;
#12904 = APPROVAL_PERSON_ORGANIZATION ( #14173, #9908, #12398 ) ;
#12905 = EDGE_LOOP ( 'NONE', ( #10325, #22774, #16950, #16127 ) ) ;
#12906 = DIRECTION ( 'NONE',  ( 3.211814849206744928E-17, -2.442368445299930211E-15, -1.000000000000000000 ) ) ;
#12907 = ORIENTED_EDGE ( 'NONE', *, *, #6029, .F. ) ;
#12909 = CONICAL_SURFACE ( 'NONE', #22748, 2.624999999999998668, 0.4636476090008128104 ) ;
#12908 = PLANE ( 'NONE',  #17016 ) ;
#12910 = ORIENTED_EDGE ( 'NONE', *, *, #6328, .F. ) ;
#12911 = AXIS2_PLACEMENT_3D ( 'NONE', #5486, #18316, #2040 ) ;
#12912 = CARTESIAN_POINT ( 'NONE',  ( -68.00125749501478367, 8.040554167933716911, 1.590559959464714451E-15 ) ) ;
#12913 = CARTESIAN_POINT ( 'NONE',  ( 28.41185834866789861, -1.882976958576060067, 13.00000000000019895 ) ) ;
#12914 = CARTESIAN_POINT ( 'NONE',  ( -19.49999999982360066, -0.1021026942259700004, -1.101737663870589950E-14 ) ) ;
#12915 = ORIENTED_EDGE ( 'NONE', *, *, #15919, .T. ) ;
#12916 = CC_DESIGN_APPROVAL ( #20557, ( #6084 ) ) ;
#12917 = DATE_TIME_ROLE ( 'classification_date' ) ;
#12918 = CARTESIAN_POINT ( 'NONE',  ( 1.406882533891259834, 17.87809865158410005, -7.060250502199809043E-15 ) ) ;
#12919 = APPROVAL_PERSON_ORGANIZATION ( #12588, #1680, #12810 ) ;
#12920 = ORIENTED_EDGE ( 'NONE', *, *, #5597, .T. ) ;
#12921 = COORDINATED_UNIVERSAL_TIME_OFFSET ( 0, 0, .AHEAD. ) ;
#12922 = EDGE_LOOP ( 'NONE', ( #958, #19437, #5045, #18388 ) ) ;
#12923 = ORIENTED_EDGE ( 'NONE', *, *, #14381, .T. ) ;
#12924 = DIRECTION ( 'NONE',  ( 3.210834492194360164E-17, -2.441916418604790135E-15, -1.000000000000000000 ) ) ;
#12925 = PERSON_AND_ORGANIZATION_ROLE ( 'creator' ) ;
#12926 = AXIS2_PLACEMENT_3D ( 'NONE', #22623, #771, #7922 ) ;
#12927 = CARTESIAN_POINT ( 'NONE',  ( 39.27359436029389883, 22.26288585089424998, -13.00000000000030020 ) ) ;
#12928 = APPROVAL_DATE_TIME ( #21715, #9960 ) ;
#12929 = CARTESIAN_POINT ( 'NONE',  ( -0.03403376487617940094, 6.499910899608420500, -8.889172688581379631E-14 ) ) ;
#12930 = EDGE_CURVE ( 'NONE', #8934, #16466, #14746, .T. ) ;
#12931 = APPROVAL_PERSON_ORGANIZATION ( #15899, #6196, #23126 ) ;
#12932 =( NAMED_UNIT ( * ) SI_UNIT ( $, .STERADIAN. ) SOLID_ANGLE_UNIT ( ) );
#12933 = SECURITY_CLASSIFICATION ( '', '', #16288 ) ;
#12934 = FACE_OUTER_BOUND ( 'NONE', #7600, .T. ) ;
#12935 = VECTOR ( 'NONE', #4241, 999.9999999999998863 ) ;
#12936 = CALENDAR_DATE ( 2026, 31, 10 ) ;
#12937 = ORIENTED_EDGE ( 'NONE', *, *, #16282, .T. ) ;
#12938 = CC_DESIGN_SECURITY_CLASSIFICATION ( #12227, ( #23493 ) ) ;
#12939 = LINE ( 'NONE', #16970, #4063 ) ;
#12940 = AXIS2_PLACEMENT_3D ( 'NONE', #17026, #8142, #4343 ) ;
#12941 = ORIENTED_EDGE ( 'NONE', *, *, #6334, .F. ) ;
#12942 = DIRECTION ( 'NONE',  ( 0.6862566701892842680, 0.7273594590164591533, -3.576853004787541598E-15 ) ) ;
#12943 = DIRECTION ( 'NONE',  ( -2.269747459788994803E-13, -2.220446049250330436E-15, -1.000000000000000000 ) ) ;
#12944 = CARTESIAN_POINT ( 'NONE',  ( -57.73978104676354661, -25.30277024906005678, -5.538318824519921191E-15 ) ) ;
#12945 = VERTEX_POINT ( 'NONE', #14977 ) ;
#12946 = EDGE_LOOP ( 'NONE', ( #14258, #12185, #13528, #18427 ) ) ;
#12947 = FACE_OUTER_BOUND ( 'NONE', #16827, .T. ) ;
#12948 = VERTEX_POINT ( 'NONE', #358 ) ;
#12949 = PERSON_AND_ORGANIZATION ( #11966, #8758 ) ;
#12950 = CC_DESIGN_APPROVAL ( #2542, ( #6135 ) ) ;
#12951 = ORIENTED_EDGE ( 'NONE', *, *, #5222, .F. ) ;
#12952 = ORIENTED_EDGE ( 'NONE', *, *, #8760, .T. ) ;
#12953 = PLANE ( 'NONE',  #5022 ) ;
#12954 = APPROVAL_PERSON_ORGANIZATION ( #9030, #22338, #7140 ) ;
#12955 = DIRECTION ( 'NONE',  ( 1.000000000000000000, 0.000000000000000000, 0.000000000000000000 ) ) ;
#12956 = COORDINATED_UNIVERSAL_TIME_OFFSET ( 0, 0, .AHEAD. ) ;
#12957 = VECTOR ( 'NONE', #8187, 999.9999999999998863 ) ;
#12958 = FACE_BOUND ( 'NONE', #1115, .T. ) ;
#12959 = VECTOR ( 'NONE', #4898, 1000.000000000000000 ) ;
#12960 = CARTESIAN_POINT ( 'NONE',  ( 117.1241794131700118, -12.63305097454420078, 15.50000000000000000 ) ) ;
#12961 = LOCAL_TIME ( 14, 11, 27.00000000000000000, #12903 ) ;
#12962 = EDGE_CURVE ( 'NONE', #21440, #15675, #9530, .T. ) ;
#12963 = ADVANCED_FACE ( 'NONE', ( #18324, #21972 ), #239, .F. ) ;
#12964 = EDGE_LOOP ( 'NONE', ( #18064, #22898, #7151, #19239 ) ) ;
#12965 = CARTESIAN_POINT ( 'NONE',  ( 34.49867763533223552, 5.152869186095713872, -26.88000000000047507 ) ) ;
#12966 = PERSON_AND_ORGANIZATION ( #11966, #8758 ) ;
#12967 = CC_DESIGN_APPROVAL ( #15623, ( #6911 ) ) ;
#12968 = ORIENTED_EDGE ( 'NONE', *, *, #3956, .F. ) ;
#12969 = CIRCLE ( 'NONE', #7284, 3.750000000000000000 ) ;
#12970 = CARTESIAN_POINT ( 'NONE',  ( -20.00000000397080058, 22.95208919256900160, 8.500000000004460432 ) ) ;
#12971 = EDGE_CURVE ( 'NONE', #15644, #21038, #15096, .T. ) ;
#12972 = ADVANCED_FACE ( 'NONE', ( #5846 ), #18444, .T. ) ;
#12973 = CARTESIAN_POINT ( 'NONE',  ( -14.54830929634010062, -2.787889851644890005, -7.999999999996738609 ) ) ;
#12974 = CARTESIAN_POINT ( 'NONE',  ( 5.000000000000000000, -23.36217782649100272, -2.500000000000000000 ) ) ;
#12975 = CIRCLE ( 'NONE', #19439, 2.499999999999998224 ) ;
#12976 = VECTOR ( 'NONE', #1260, 1000.000000000000227 ) ;
#12977 = DIRECTION ( 'NONE',  ( 0.000000000000000000, 0.000000000000000000, 1.000000000000000000 ) ) ;
#12978 = ORIENTED_EDGE ( 'NONE', *, *, #9493, .F. ) ;
#12979 = CC_DESIGN_APPROVAL ( #10397, ( #8052 ) ) ;
#12980 = CARTESIAN_POINT ( 'NONE',  ( 33.70449598666325386, 8.926526082478684287, 8.911899047890422310 ) ) ;
#12981 = UNCERTAINTY_MEASURE_WITH_UNIT (LENGTH_MEASURE( 1.000000000000000082E-05 ), #2012, 'distance_accuracy_value', 'NONE');
#12982 = AXIS2_PLACEMENT_3D ( 'NONE', #11226, #14872, #16766 ) ;
#12983 = VERTEX_POINT ( 'NONE', #11215 ) ;
#12984 = VERTEX_POINT ( 'NONE', #12965 ) ;
#12985 = DIRECTION ( 'NONE',  ( 0.000000000000000000, 0.000000000000000000, -1.000000000000000000 ) ) ;
#12986 = VECTOR ( 'NONE', #2254, 1000.000000000000227 ) ;
#12987 = DIRECTION ( 'NONE',  ( 6.124378941433959925E-17, 0.000000000000000000, 1.000000000000000000 ) ) ;
#12988 = ORIENTED_EDGE ( 'NONE', *, *, #15395, .F. ) ;
#12989 = PLANE ( 'NONE',  #11517 ) ;
#12990 = ORIENTED_EDGE ( 'NONE', *, *, #21135, .T. ) ;
#12991 = LOCAL_TIME ( 14, 11, 27.00000000000000000, #10587 ) ;
#12992 = DIRECTION ( 'NONE',  ( 0.9730401042858036753, -0.2306359803922031493, -5.959266323858673745E-17 ) ) ;
#12993 = DATE_AND_TIME ( #5739, #127 ) ;
#12994 = AXIS2_PLACEMENT_3D ( 'NONE', #4064, #5853, #12977 ) ;
#12995 = DIRECTION ( 'NONE',  ( 0.9822610636820822139, -0.1875185398144529336, 4.336808689942018229E-16 ) ) ;
#12996 = AXIS2_PLACEMENT_3D ( 'NONE', #17517, #19295, #12073 ) ;
#12997 = EDGE_CURVE ( 'NONE', #3813, #6789, #11724, .T. ) ;
#12998 = CIRCLE ( 'NONE', #13763, 5.000000000000001776 ) ;
#12999 = CYLINDRICAL_SURFACE ( 'NONE', #9226, 2.499999999999998668 ) ;
#13000 = CC_DESIGN_DATE_AND_TIME_ASSIGNMENT ( #15379, #22610, ( #9377 ) ) ;
#13001 = VECTOR ( 'NONE', #8019, 1000.000000000000000 ) ;
#13002 = DIRECTION ( 'NONE',  ( -0.2306359803922102825, -0.9730401042858017879, 4.163336342344335449E-15 ) ) ;
#13003 = APPROVAL_ROLE ( '' ) ;
#13004 = CC_DESIGN_PERSON_AND_ORGANIZATION_ASSIGNMENT ( #13275, #2223, ( #5355 ) ) ;
#13005 = DIRECTION ( 'NONE',  ( -1.000000000000000000, -6.662112528310618598E-09, 2.269018306577664942E-13 ) ) ;
#13006 = CIRCLE ( 'NONE', #5801, 2.500000000000000444 ) ;
#13007 = CARTESIAN_POINT ( 'NONE',  ( 31.65707447484311743, 2.486356205010289866, 13.00000000000000000 ) ) ;
#13008 = EDGE_CURVE ( 'NONE', #4824, #19473, #4055, .T. ) ;
#13009 = EDGE_CURVE ( 'NONE', #19010, #22465, #18525, .T. ) ;
#13010 = FACE_BOUND ( 'NONE', #10960, .T. ) ;
#13011 = CC_DESIGN_APPROVAL ( #5163, ( #14534 ) ) ;
#13012 = DIRECTION ( 'NONE',  ( -0.005235963827116131390, 0.9999862922474493931, 2.636227439667251184E-16 ) ) ;
#13013 = EDGE_CURVE ( 'NONE', #8336, #7018, #21533, .T. ) ;
#13015 = EDGE_CURVE ( 'NONE', #3556, #2801, #7148, .T. ) ;
#13014 = CARTESIAN_POINT ( 'NONE',  ( 52.73786095581300515, -7.648876468381270222, -15.00924000000035008 ) ) ;
#13016 = CIRCLE ( 'NONE', #22870, 5.000000000000004441 ) ;
#13017 = LINE ( 'NONE', #14431, #2360 ) ;
#13018 = VECTOR ( 'NONE', #13226, 1000.000000000000000 ) ;
#13019 = EDGE_LOOP ( 'NONE', ( #3218, #9016, #16531, #22965 ) ) ;
#13020 = EDGE_CURVE ( 'NONE', #90, #21956, #19296, .T. ) ;
#13021 = VECTOR ( 'NONE', #15933, 1000.000000000000227 ) ;
#13022 = VERTEX_POINT ( 'NONE', #9410 ) ;
#13023 = PLANE ( 'NONE',  #8458 ) ;
#13024 = DIRECTION ( 'NONE',  ( 6.123237831918399306E-17, -9.341417679122849747E-31, -1.000000000000000000 ) ) ;
#13025 = EDGE_LOOP ( 'NONE', ( #591, #5413 ) ) ;
#13026 = CARTESIAN_POINT ( 'NONE',  ( 35.93893384793820189, -10.44995626450799975, 2.700000000000000178 ) ) ;
#13027 = VERTEX_POINT ( 'NONE', #16874 ) ;
#13028 = DIRECTION ( 'NONE',  ( -1.138590270679728013E-14, -2.220446049251240387E-15, -1.000000000000000000 ) ) ;
#13029 = TOROIDAL_SURFACE ( 'NONE', #23247, 3.750000000000000000, 0.5000000000000000000 ) ;
#13030 = PERSON_AND_ORGANIZATION_ROLE ( 'design_supplier' ) ;
#13031 = DIRECTION ( 'NONE',  ( 0.000000000000000000, 0.000000000000000000, -1.000000000000000000 ) ) ;
#13032 = EDGE_CURVE ( 'NONE', #16843, #9845, #132, .T. ) ;
#13033 = CC_DESIGN_SECURITY_CLASSIFICATION ( #18743, ( #23475 ) ) ;
#13034 = COORDINATED_UNIVERSAL_TIME_OFFSET ( 0, 0, .AHEAD. ) ;
#13035 = AXIS2_PLACEMENT_3D ( 'NONE', #278, #8879, #7201 ) ;
#13036 = CARTESIAN_POINT ( 'NONE',  ( 1.406882533891259834, 17.87809865158410005, -7.060250502199809043E-15 ) ) ;
#13037 = VECTOR ( 'NONE', #15818, 1000.000000000000000 ) ;
#13038 = ORIENTED_EDGE ( 'NONE', *, *, #18074, .T. ) ;
#13039 = PERSON ( 'NAUO-PER28', 'UNSPECIFIED', 'UNSPECIFIED', ('UNSPECIFIED'), ('UNSPECIFIED'), ('UNSPECIFIED') ) ;
#13040 = DIRECTION ( 'NONE',  ( 0.005235963827117092427, -0.9999862922474493931, -2.636227439667000721E-16 ) ) ;
#13041 = ORIENTED_EDGE ( 'NONE', *, *, #2258, .T. ) ;
#13042 = CARTESIAN_POINT ( 'NONE',  ( -11.24263882182209962, 20.87636639668270178, -8.642052169251309479 ) ) ;
#13043 = EDGE_CURVE ( 'NONE', #10377, #18172, #10209, .T. ) ;
#13044 = EDGE_CURVE ( 'NONE', #2445, #1396, #10971, .T. ) ;
#13045 = CARTESIAN_POINT ( 'NONE',  ( -67.06978017061331343, -25.35162245663349978, 2.500000000000000000 ) ) ;
#13046 = ORIENTED_EDGE ( 'NONE', *, *, #22449, .F. ) ;
#13047 = VECTOR ( 'NONE', #19966, 1000.000000000000114 ) ;
#13048 = LINE ( 'NONE', #20162, #16544 ) ;
#13049 = FACE_OUTER_BOUND ( 'NONE', #10604, .T. ) ;
#13050 = DIRECTION ( 'NONE',  ( 1.000000000000000000, 0.000000000000000000, 0.000000000000000000 ) ) ;
#13051 = ORIENTED_EDGE ( 'NONE', *, *, #4384, .F. ) ;
#13052 = AXIS2_PLACEMENT_3D ( 'NONE', #14227, #4846, #3189 ) ;
#13053 = ITEM_DEFINED_TRANSFORMATION ( 'NONE', 'NONE', #18595,  #12739 ) ;
#13054 = CARTESIAN_POINT ( 'NONE',  ( 36.17078849317572065, 12.20740994216797404, 10.99076000000018816 ) ) ;
#13055 = AXIS2_PLACEMENT_3D ( 'NONE', #11422, #18655, #9643 ) ;
#13056 = EDGE_LOOP ( 'NONE', ( #1158, #21020, #1818, #7530 ) ) ;
#13057 = PERSON_AND_ORGANIZATION ( #11966, #8758 ) ;
#13058 = DIRECTION ( 'NONE',  ( -1.000000000000000000, 0.000000000000000000, -0.000000000000000000 ) ) ;
#13059 = ORIENTED_EDGE ( 'NONE', *, *, #9558, .F. ) ;
#13060 = ORIENTED_EDGE ( 'NONE', *, *, #6434, .T. ) ;
#13061 = PERSON_AND_ORGANIZATION ( #11966, #8758 ) ;
#13062 = EDGE_CURVE ( 'NONE', #22391, #20016, #3409, .T. ) ;
#13063 = CARTESIAN_POINT ( 'NONE',  ( 36.88454136754619128, -6.460491836936199661, 3.000000000000000000 ) ) ;
#13064 = DATE_TIME_ROLE ( 'classification_date' ) ;
#13065 = DIRECTION ( 'NONE',  ( 0.2306359803922076457, 0.9730401042858023430, 0.000000000000000000 ) ) ;
#13066 = AXIS2_PLACEMENT_3D ( 'NONE', #6103, #4089, #869 ) ;
#13067 = SHAPE_REPRESENTATION_RELATIONSHIP ( 'NONE' , 'NONE' ,  #12508, #865 ) ;
#13068 = EDGE_CURVE ( 'NONE', #5571, #2641, #4504, .T. ) ;
#13069 = DIRECTION ( 'NONE',  ( 0.000000000000000000, 0.000000000000000000, 1.000000000000000000 ) ) ;
#13070 = AXIS2_PLACEMENT_3D ( 'NONE', #13996, #21121, #10577 ) ;
#13071 = EDGE_CURVE ( 'NONE', #1739, #19931, #12460, .T. ) ;
#13072 = APPROVAL_ROLE ( '' ) ;
#13073 = EDGE_CURVE ( 'NONE', #12469, #8919, #15441, .T. ) ;
#13074 = ORIENTED_EDGE ( 'NONE', *, *, #977, .F. ) ;
#13075 = CARTESIAN_POINT ( 'NONE',  ( -20.00019857044559757, 22.95165872133759777, -2.500000000000059952 ) ) ;
#13076 = EDGE_LOOP ( 'NONE', ( #9071, #7818, #7936, #1431, #2581, #21201 ) ) ;
#13077 = FACE_BOUND ( 'NONE', #7721, .T. ) ;
#13078 = CARTESIAN_POINT ( 'NONE',  ( -66.29618031796869104, -0.3471291603817610039, -5.500000000000079048 ) ) ;
#13079 = ORIENTED_EDGE ( 'NONE', *, *, #15900, .T. ) ;
#13080 = ORIENTED_EDGE ( 'NONE', *, *, #12616, .T. ) ;
#13081 = DIRECTION ( 'NONE',  ( 1.000000000000000000, 2.982858504577319616E-17, 8.758115402030109610E-48 ) ) ;
#13082 = VERTEX_POINT ( 'NONE', #7981 ) ;
#13083 = PERSON_AND_ORGANIZATION_ROLE ( 'creator' ) ;
#13084 = VERTEX_POINT ( 'NONE', #4760 ) ;
#13085 = VERTEX_POINT ( 'NONE', #17358 ) ;
#13086 = CARTESIAN_POINT ( 'NONE',  ( 28.89837840081079889, -1.998294948772289858, -13.00000000000039968 ) ) ;
#13087 = CARTESIAN_POINT ( 'NONE',  ( 28.03349347434003747, -5.647195339843935180, 13.00000000000019895 ) ) ;
#13088 = CALENDAR_DATE ( 2026, 31, 10 ) ;
#13089 = APPLICATION_CONTEXT ( 'configuration controlled 3d designs of mechanical parts and assemblies' ) ;
#13090 = DIRECTION ( 'NONE',  ( 0.000000000000000000, 0.000000000000000000, 1.000000000000000000 ) ) ;
#13091 = DIRECTION ( 'NONE',  ( -0.9999862922474491711, -0.005235963827128302210, 1.187304881134281446E-16 ) ) ;
#13092 = CC_DESIGN_PERSON_AND_ORGANIZATION_ASSIGNMENT ( #21515, #17740, ( #796 ) ) ;
#13093 =( LENGTH_UNIT ( ) NAMED_UNIT ( * ) SI_UNIT ( .MILLI., .METRE. ) );
#13094 = ORIENTED_EDGE ( 'NONE', *, *, #14132, .T. ) ;
#13095 = CARTESIAN_POINT ( 'NONE',  ( -20.00000000397360012, 22.95208919256889857, -2.500000000000039968 ) ) ;
#13096 = COORDINATED_UNIVERSAL_TIME_OFFSET ( 0, 0, .AHEAD. ) ;
#13097 = VECTOR ( 'NONE', #3774, 1000.000000000000114 ) ;
#13098 = ORIENTED_EDGE ( 'NONE', *, *, #16450, .T. ) ;
#13099 = CARTESIAN_POINT ( 'NONE',  ( -29.94170640616770029, 6.343313258985349812, -2.500000000000000000 ) ) ;
#13100 = DIRECTION ( 'NONE',  ( -6.662111519016958720E-09, 1.000000000000000000, -2.523234146875356491E-15 ) ) ;
#13101 = FACE_OUTER_BOUND ( 'NONE', #1285, .T. ) ;
#13102 = LINE ( 'NONE', #8115, #18305 ) ;
#13103 = ORIENTED_EDGE ( 'NONE', *, *, #6234, .T. ) ;
#13104 = CARTESIAN_POINT ( 'NONE',  ( 117.1933702072879981, -12.34113894325849969, -18.89999999999999858 ) ) ;
#13105 = DATE_AND_TIME ( #2764, #2681 ) ;
#13106 = EDGE_CURVE ( 'NONE', #21398, #13515, #1834, .T. ) ;
#13107 = PRODUCT ( '1602p_c_11', '1602p_c_11', '', ( #14596 ) ) ;
#13108 = EDGE_LOOP ( 'NONE', ( #21475, #22305, #9710, #17034 ) ) ;
#13109 = EDGE_LOOP ( 'NONE', ( #7238, #17714, #1066, #14357 ) ) ;
#13110 = CYLINDRICAL_SURFACE ( 'NONE', #12269, 4.999999999999996447 ) ;
#13111 = CARTESIAN_POINT ( 'NONE',  ( -31.64153798721130428, 6.334539654120280083, 5.000000000000000000 ) ) ;
#13112 = ORIENTED_EDGE ( 'NONE', *, *, #2425, .T. ) ;
#13113 = PERSON_AND_ORGANIZATION_ROLE ( 'classification_officer' ) ;
#13114 = CARTESIAN_POINT ( 'NONE',  ( 58.25686728443110241, 17.76335315678750248, 13.00000000000000000 ) ) ;
#13115 = CIRCLE ( 'NONE', #6675, 2.500000000000000000 ) ;
#13116 = CARTESIAN_POINT ( 'NONE',  ( -18.05391955182270181, 22.49081825942809942, -4.900728725074969882E-15 ) ) ;
#13117 = DATE_TIME_ROLE ( 'classification_date' ) ;
#13118 = CARTESIAN_POINT ( 'NONE',  ( 33.91471097434134663, 19.16532731944453616, 13.00000000000000000 ) ) ;
#13119 = EDGE_CURVE ( 'NONE', #1694, #8933, #8684, .T. ) ;
#13120 = LINE ( 'NONE', #270, #1629 ) ;
#13121 = CARTESIAN_POINT ( 'NONE',  ( -17.50000000000000000, -19.99999998334472195, 5.500000000004530598 ) ) ;
#13122 = CALENDAR_DATE ( 2026, 31, 10 ) ;
#13123 = DIRECTION ( 'NONE',  ( -2.982858504577319616E-17, 2.441916418604790135E-15, 1.000000000000000000 ) ) ;
#13124 = CARTESIAN_POINT ( 'NONE',  ( 31.11077410011089839, -1.335996977273150144, 15.00000000000000000 ) ) ;
#13125 = CARTESIAN_POINT ( 'NONE',  ( 114.8732178155626826, -20.25231274233364687, -13.00000000000000000 ) ) ;
#13126 = AXIS2_PLACEMENT_3D ( 'NONE', #6939, #5250, #1329 ) ;
#13127 = LINE ( 'NONE', #4557, #5735 ) ;
#13128 = LINE ( 'NONE', #10250, #13422 ) ;
#13129 = LINE ( 'NONE', #528, #5797 ) ;
#13130 = VERTEX_POINT ( 'NONE', #8105 ) ;
#13131 = CIRCLE ( 'NONE', #17684, 2.750000000000001332 ) ;
#13132 = EDGE_CURVE ( 'NONE', #7550, #2884, #4647, .T. ) ;
#13133 = VERTEX_POINT ( 'NONE', #6419 ) ;
#13134 = CARTESIAN_POINT ( 'NONE',  ( 35.59419854219520118, 9.774809681453278998, 25.00000000000000000 ) ) ;
#13135 = FACE_OUTER_BOUND ( 'NONE', #21156, .T. ) ;
#13136 = ORIENTED_EDGE ( 'NONE', *, *, #13332, .F. ) ;
#13137 = CC_DESIGN_PERSON_AND_ORGANIZATION_ASSIGNMENT ( #204, #14362, ( #9089 ) ) ;
#13138 = CARTESIAN_POINT ( 'NONE',  ( -69.83648240813079155, -6.865755409778350860, -7.200000000000000178 ) ) ;
#13139 = ORIENTED_EDGE ( 'NONE', *, *, #22024, .T. ) ;
#13140 = COORDINATED_UNIVERSAL_TIME_OFFSET ( 0, 0, .AHEAD. ) ;
#13141 = CARTESIAN_POINT ( 'NONE',  ( 37.66476571482293423, 9.834146374661965950, -8.985048276826022473 ) ) ;
#13142 = EDGE_CURVE ( 'NONE', #560, #6915, #21936, .T. ) ;
#13143 = EDGE_CURVE ( 'NONE', #20578, #11097, #20961, .T. ) ;
#13144 = CIRCLE ( 'NONE', #18850, 2.750000000000002220 ) ;
#13145 = APPROVAL_DATE_TIME ( #15270, #5436 ) ;
#13146 = AXIS2_PLACEMENT_3D ( 'NONE', #11956, #4555, #8249 ) ;
#13147 = FACE_OUTER_BOUND ( 'NONE', #2477, .T. ) ;
#13148 = EDGE_LOOP ( 'NONE', ( #2111, #17094, #10176, #6027 ) ) ;
#13149 = DIRECTION ( 'NONE',  ( 0.000000000000000000, -1.000000000000000000, 4.969341027148640384E-15 ) ) ;
#13150 = ORIENTED_EDGE ( 'NONE', *, *, #4480, .T. ) ;
#13151 = LINE ( 'NONE', #22388, #5980 ) ;
#13152 = CARTESIAN_POINT ( 'NONE',  ( -24.50000000000000000, -31.09999999999999787, -21.50000000000000000 ) ) ;
#13153 = ORIENTED_EDGE ( 'NONE', *, *, #15197, .T. ) ;
#13154 = DIRECTION ( 'NONE',  ( 0.005235963827121942714, -0.9999862922474493931, -2.738609489598291197E-14 ) ) ;
#13155 = DIRECTION ( 'NONE',  ( -2.982858504577249974E-17, 2.441916418604790135E-15, 1.000000000000000000 ) ) ;
#13156 = CARTESIAN_POINT ( 'NONE',  ( -22.99995202268987171, -0.1204285676208978334, 9.211416015219178562E-14 ) ) ;
#13157 = EDGE_LOOP ( 'NONE', ( #7468, #13915 ) ) ;
#13158 = ADVANCED_FACE ( 'NONE', ( #20906 ), #15213, .F. ) ;
#13159 = AXIS2_PLACEMENT_3D ( 'NONE', #20491, #411, #11263 ) ;
#13160 = CONTEXT_DEPENDENT_SHAPE_REPRESENTATION ( #15047, #5681 ) ;
#13161 = VECTOR ( 'NONE', #10574, 1000.000000000000000 ) ;
#13162 = DIRECTION ( 'NONE',  ( 0.000000000000000000, -6.936119456125000933E-16, -1.000000000000000000 ) ) ;
#13163 = CIRCLE ( 'NONE', #20746, 4.250000000000001776 ) ;
#13164 = EDGE_LOOP ( 'NONE', ( #12208, #10700, #8025, #18781, #21206, #16807 ) ) ;
#13166 = PERSON_AND_ORGANIZATION ( #11966, #8758 ) ;
#13165 = PRODUCT_DEFINITION ( 'UNKNOWN', '', #7661, #10655 ) ;
#13167 = DIRECTION ( 'NONE',  ( -2.312964634635742957E-16, 0.000000000000000000, 1.000000000000000000 ) ) ;
#13168 = ORIENTED_EDGE ( 'NONE', *, *, #13751, .F. ) ;
#13169 = ORIENTED_EDGE ( 'NONE', *, *, #18253, .T. ) ;
#13170 = CC_DESIGN_DATE_AND_TIME_ASSIGNMENT ( #3793, #10729, ( #3714 ) ) ;
#13171 = CARTESIAN_POINT ( 'NONE',  ( 35.59419854219520118, 9.774809681453278998, 21.49999999999999289 ) ) ;
#13172 = CALENDAR_DATE ( 2026, 31, 10 ) ;
#13173 = EDGE_CURVE ( 'NONE', #21550, #15073, #2973, .T. ) ;
#13174 = ADVANCED_FACE ( 'NONE', ( #22799 ), #2749, .F. ) ;
#13175 = COORDINATED_UNIVERSAL_TIME_OFFSET ( 0, 0, .AHEAD. ) ;
#13176 = AXIS2_PLACEMENT_3D ( 'NONE', #7173, #21519, #248 ) ;
#13177 = CARTESIAN_POINT ( 'NONE',  ( 35.84667945578009807, -10.83917230622375882, -20.00000000000000000 ) ) ;
#13178 = VECTOR ( 'NONE', #22968, 1000.000000000000000 ) ;
#13179 = DIRECTION ( 'NONE',  ( 0.000000000000000000, 0.000000000000000000, -1.000000000000000000 ) ) ;
#13180 = APPROVAL_STATUS ( 'not_yet_approved' ) ;
#13181 = ORIENTED_EDGE ( 'NONE', *, *, #3395, .T. ) ;
#13182 = AXIS2_PLACEMENT_3D ( 'NONE', #17015, #6442, #6579 ) ;
#13183 = DIRECTION ( 'NONE',  ( 0.000000000000000000, 0.000000000000000000, -1.000000000000000000 ) ) ;
#13184 = ORIENTED_EDGE ( 'NONE', *, *, #13522, .F. ) ;
#13185 = ADVANCED_FACE ( 'NONE', ( #19024 ), #6549, .T. ) ;
#13186 = DIRECTION ( 'NONE',  ( 0.000000000000000000, 0.000000000000000000, -1.000000000000000000 ) ) ;
#13187 = CARTESIAN_POINT ( 'NONE',  ( 114.2412296582679971, -24.79605227811680379, 3.000000000000000000 ) ) ;
#13188 = CARTESIAN_POINT ( 'NONE',  ( -60.02994014102380049, 8.478793778983318319, 5.000000000000000000 ) ) ;
#13189 = AXIS2_PLACEMENT_3D ( 'NONE', #6681, #10026, #14026 ) ;
#13190 = VERTEX_POINT ( 'NONE', #6202 ) ;
#13191 = ORIENTED_EDGE ( 'NONE', *, *, #19813, .T. ) ;
#13192 = DIRECTION ( 'NONE',  ( 0.9999862922474493931, 0.005235963827108152530, 0.000000000000000000 ) ) ;
#13193 = VERTEX_POINT ( 'NONE', #10239 ) ;
#13194 = APPROVAL_ROLE ( '' ) ;
#13195 = AXIS2_PLACEMENT_3D ( 'NONE', #43, #11128, #275 ) ;
#13196 = EDGE_CURVE ( 'NONE', #2666, #13324, #6405, .T. ) ;
#13197 = AXIS2_PLACEMENT_3D ( 'NONE', #1205, #13349, #20705 ) ;
#13198 = VERTEX_POINT ( 'NONE', #11792 ) ;
#13199 = ORIENTED_EDGE ( 'NONE', *, *, #13730, .F. ) ;
#13200 = CARTESIAN_POINT ( 'NONE',  ( 122.4288069621910040, 9.746871424029301068, 13.00000000000000000 ) ) ;
#13201 = CIRCLE ( 'NONE', #20020, 3.499999999999999112 ) ;
#13202 = FACE_BOUND ( 'NONE', #4291, .T. ) ;
#13203 = APPROVAL_ROLE ( '' ) ;
#13204 = EDGE_CURVE ( 'NONE', #21046, #19719, #22564, .T. ) ;
#13205 = FACE_OUTER_BOUND ( 'NONE', #18044, .T. ) ;
#13206 = EDGE_CURVE ( 'NONE', #9676, #21726, #7164, .T. ) ;
#13207 = DIRECTION ( 'NONE',  ( 0.000000000000000000, 0.000000000000000000, 1.000000000000000000 ) ) ;
#13208 = AXIS2_PLACEMENT_3D ( 'NONE', #1381, #8647, #7103 ) ;
#13209 = VECTOR ( 'NONE', #17180, 1000.000000000000000 ) ;
#13210 = ORIENTED_EDGE ( 'NONE', *, *, #1560, .T. ) ;
#13211 = DIRECTION ( 'NONE',  ( 0.000000000000000000, 0.000000000000000000, 1.000000000000000000 ) ) ;
#13212 = DATE_AND_TIME ( #21865, #23161 ) ;
#13213 = VECTOR ( 'NONE', #5490, 1000.000000000000227 ) ;
#13214 = ORIENTED_EDGE ( 'NONE', *, *, #13299, .T. ) ;
#13215 = CARTESIAN_POINT ( 'NONE',  ( 28.88391017762861424, 3.143668749128058604, 13.00000000000000000 ) ) ;
#13216 = DIRECTION ( 'NONE',  ( 0.9730401042858036753, -0.2306359803922031493, -5.432877459303553216E-17 ) ) ;
#13217 = VERTEX_POINT ( 'NONE', #20790 ) ;
#13218 = DIRECTION ( 'NONE',  ( 0.9730401042858036753, -0.2306359803922028995, -5.432877459303547669E-17 ) ) ;
#13219 = DIRECTION ( 'NONE',  ( -0.04564792618501069266, -0.9989575901083128651, 2.775557561562892534E-15 ) ) ;
#13220 = ORIENTED_EDGE ( 'NONE', *, *, #10567, .F. ) ;
#13221 = CARTESIAN_POINT ( 'NONE',  ( -20.00000000397270128, 22.95208919257349933, 5.500000000004459544 ) ) ;
#13222 = CC_DESIGN_DATE_AND_TIME_ASSIGNMENT ( #21254, #16034, ( #1591 ) ) ;
#13223 = APPLICATION_PROTOCOL_DEFINITION ( 'international standard', 'config_control_design', 1994, #18393 ) ;
#13224 = EDGE_LOOP ( 'NONE', ( #14125, #19532, #18786, #15216 ) ) ;
#13225 = EDGE_LOOP ( 'NONE', ( #6802, #11522, #11206, #7045 ) ) ;
#13226 = DIRECTION ( 'NONE',  ( 5.964507377817269296E-17, 4.861311874385510251E-15, 1.000000000000000000 ) ) ;
#13227 = FACE_OUTER_BOUND ( 'NONE', #4144, .T. ) ;
#13228 = ORIENTED_EDGE ( 'NONE', *, *, #15657, .T. ) ;
#13229 = PERSON_AND_ORGANIZATION ( #11966, #8758 ) ;
#13230 = DIRECTION ( 'NONE',  ( 1.320147222947482081E-46, -2.155962677239134989E-30, -1.000000000000000000 ) ) ;
#13231 = DIRECTION ( 'NONE',  ( 6.123237831918399306E-17, -1.569224110909209817E-30, -1.000000000000000000 ) ) ;
#13232 = VECTOR ( 'NONE', #9005, 1000.000000000000000 ) ;
#13233 = APPROVAL_DATE_TIME ( #12993, #2233 ) ;
#13234 = CARTESIAN_POINT ( 'NONE',  ( -19.99975861755300244, 22.95209442650120124, 4.999999999999900524 ) ) ;
#13235 = LINE ( 'NONE', #5336, #20227 ) ;
#13236 = EDGE_CURVE ( 'NONE', #489, #7436, #16349, .T. ) ;
#13237 = PERSON_AND_ORGANIZATION_ROLE ( 'creator' ) ;
#13238 = FACE_OUTER_BOUND ( 'NONE', #17261, .T. ) ;
#13239 = CARTESIAN_POINT ( 'NONE',  ( 33.90884364377009774, 10.17428291754599989, -27.69000000000049866 ) ) ;
#13240 = DIRECTION ( 'NONE',  ( 0.000000000000000000, 0.000000000000000000, -1.000000000000000000 ) ) ;
#13241 = DIRECTION ( 'NONE',  ( 2.270069654138870255E-15, 1.000000000000000000, 7.035747901516317327E-77 ) ) ;
#13242 = DIRECTION ( 'NONE',  ( -0.6944962871189167553, 0.7194962871190087039, 0.000000000000000000 ) ) ;
#13243 = ORIENTED_EDGE ( 'NONE', *, *, #14874, .F. ) ;
#13244 = ORIENTED_EDGE ( 'NONE', *, *, #7942, .T. ) ;
#13245 = FACE_BOUND ( 'NONE', #21521, .T. ) ;
#13246 = CARTESIAN_POINT ( 'NONE',  ( 2.499999999999970246, -30.47499999999999787, 19.00000000000000000 ) ) ;
#13247 = ORIENTED_EDGE ( 'NONE', *, *, #4774, .F. ) ;
#13248 = CIRCLE ( 'NONE', #3001, 2.500000000000000000 ) ;
#13249 = FACE_OUTER_BOUND ( 'NONE', #1487, .T. ) ;
#13250 = ORIENTED_EDGE ( 'NONE', *, *, #12191, .F. ) ;
#13251 = CYLINDRICAL_SURFACE ( 'NONE', #19636, 3.499999999999998668 ) ;
#13252 = APPROVAL_ROLE ( '' ) ;
#13253 = LINE ( 'NONE', #541, #23002 ) ;
#13254 = DATE_AND_TIME ( #20496, #14099 ) ;
#13255 =( NAMED_UNIT ( * ) PLANE_ANGLE_UNIT ( ) SI_UNIT ( $, .RADIAN. ) );
#13256 =( REPRESENTATION_RELATIONSHIP ('NONE','NONE', #18121, #10092 ) REPRESENTATION_RELATIONSHIP_WITH_TRANSFORMATION ( #10564 )SHAPE_REPRESENTATION_RELATIONSHIP( ) );
#13257 = DIRECTION ( 'NONE',  ( -0.2306359803922028440, -0.9730401042858034533, -4.307366329831518561E-32 ) ) ;
#13258 = ORIENTED_EDGE ( 'NONE', *, *, #11027, .T. ) ;
#13259 = EDGE_CURVE ( 'NONE', #5830, #20452, #18148, .T. ) ;
#13260 = ORGANIZATION ( 'NAUO-ORG10', 'UNSPECIFIED', 'UNSPECIFIED' ) ;
#13261 = LINE ( 'NONE', #16934, #20994 ) ;
#13262 = VECTOR ( 'NONE', #5384, 1000.000000000000000 ) ;
#13263 = ORIENTED_EDGE ( 'NONE', *, *, #23032, .F. ) ;
#13264 = CARTESIAN_POINT ( 'NONE',  ( -20.00000002145907274, 25.57708919256899804, 8.250000000004455103 ) ) ;
#13265 = DIRECTION ( 'NONE',  ( -0.9730401042858035643, 0.2306359803922028717, 6.126766849694256332E-17 ) ) ;
#13266 = EDGE_LOOP ( 'NONE', ( #15423, #5822, #20018, #13569, #9217 ) ) ;
#13267 = CARTESIAN_POINT ( 'NONE',  ( 35.93893384793820189, -10.44995626450799975, -2.700000000000000178 ) ) ;
#13268 = LINE ( 'NONE', #15515, #12935 ) ;
#13269 = EDGE_LOOP ( 'NONE', ( #14927, #18125, #4415, #4275 ) ) ;
#13270 = EDGE_CURVE ( 'NONE', #8287, #3632, #7112, .T. ) ;
#13271 = EDGE_CURVE ( 'NONE', #11012, #22086, #7547, .T. ) ;
#13272 = APPROVAL_ROLE ( '' ) ;
#13273 = CARTESIAN_POINT ( 'NONE',  ( -67.73964396923804543, -25.35512988733119855, 1.339745962155619363 ) ) ;
#13274 = EDGE_LOOP ( 'NONE', ( #16688, #12671, #6632, #4430, #18066, #5442, #9239, #4746 ) ) ;
#13275 = PERSON_AND_ORGANIZATION ( #11966, #8758 ) ;
#13276 = LINE ( 'NONE', #6272, #2744 ) ;
#13277 = ADVANCED_FACE ( 'NONE', ( #9114 ), #14343, .T. ) ;
#13278 = ORIENTED_EDGE ( 'NONE', *, *, #15198, .F. ) ;
#13279 = ORIENTED_EDGE ( 'NONE', *, *, #22977, .T. ) ;
#13280 = DIRECTION ( 'NONE',  ( -3.210834492181045054E-17, 2.441916418604790135E-15, 1.000000000000000000 ) ) ;
#13281 = DATE_AND_TIME ( #8059, #13756 ) ;
#13282 = AXIS2_PLACEMENT_3D ( 'NONE', #7843, #21955, #2132 ) ;
#13283 = COORDINATED_UNIVERSAL_TIME_OFFSET ( 0, 0, .AHEAD. ) ;
#13284 = CARTESIAN_POINT ( 'NONE',  ( 120.8143550994449953, 2.935590694028659797, 13.00000000000000000 ) ) ;
#13285 = ADVANCED_FACE ( 'NONE', ( #3539 ), #7567, .T. ) ;
#13286 = AXIS2_PLACEMENT_3D ( 'NONE', #5021, #1681, #16062 ) ;
#13287 = DIRECTION ( 'NONE',  ( -0.9730401042858022320, 0.2306359803922080343, 5.959266323858941219E-17 ) ) ;
#13288 = VERTEX_POINT ( 'NONE', #301 ) ;
#13289 = CC_DESIGN_PERSON_AND_ORGANIZATION_ASSIGNMENT ( #15997, #16338, ( #4302 ) ) ;
#13290 = EDGE_CURVE ( 'NONE', #2844, #15962, #18031, .T. ) ;
#13291 = PERSON_AND_ORGANIZATION ( #11966, #8758 ) ;
#13292 = PRODUCT ( '1602p_c_06', '1602p_c_06', '', ( #7821 ) ) ;
#13293 = CC_DESIGN_SECURITY_CLASSIFICATION ( #11807, ( #21633 ) ) ;
#13294 = CC_DESIGN_PERSON_AND_ORGANIZATION_ASSIGNMENT ( #15053, #16586, ( #6120 ) ) ;
#13295 = ORIENTED_EDGE ( 'NONE', *, *, #21861, .F. ) ;
#13296 = LINE ( 'NONE', #20420, #9163 ) ;
#13297 = ORIENTED_EDGE ( 'NONE', *, *, #16219, .F. ) ;
#13298 = ADVANCED_FACE ( 'NONE', ( #1627 ), #21573, .F. ) ;
#13299 = EDGE_CURVE ( 'NONE', #9680, #11640, #318, .T. ) ;
#13300 = CARTESIAN_POINT ( 'NONE',  ( -22.49917142882856069, 22.89791325974001879, 3.749999999999900080 ) ) ;
#13301 = CC_DESIGN_PERSON_AND_ORGANIZATION_ASSIGNMENT ( #14714, #14604, ( #6843 ) ) ;
#13302 = DIRECTION ( 'NONE',  ( -0.9730401042858024541, 0.2306359803922080898, 5.959266323858942451E-17 ) ) ;
#13303 = CARTESIAN_POINT ( 'NONE',  ( 53.15246078658950069, 27.48624099592299785, 3.293763653412249631E-14 ) ) ;
#13304 = VERTEX_POINT ( 'NONE', #185 ) ;
#13305 = VERTEX_POINT ( 'NONE', #7452 ) ;
#13306 = CARTESIAN_POINT ( 'NONE',  ( 77.95761363658371579, -13.11276471035541213, 3.659235858378048644E-14 ) ) ;
#13307 = ORIENTED_EDGE ( 'NONE', *, *, #15333, .F. ) ;
#13308 = CIRCLE ( 'NONE', #8764, 7.599342076785325695 ) ;
#13309 = DATE_AND_TIME ( #466, #18227 ) ;
#13310 = ORIENTED_EDGE ( 'NONE', *, *, #8995, .F. ) ;
#13311 = EDGE_LOOP ( 'NONE', ( #21572, #10004 ) ) ;
#13312 = DIRECTION ( 'NONE',  ( -0.9730401042858035643, 0.2306359803922028717, 6.126766849694256332E-17 ) ) ;
#13313 = PERSON_AND_ORGANIZATION ( #11966, #8758 ) ;
#13314 = CARTESIAN_POINT ( 'NONE',  ( -19.99999999999809930, -20.00000000000000000, 8.500000000004551026 ) ) ;
#13315 = APPROVAL_PERSON_ORGANIZATION ( #6433, #11882, #1546 ) ;
#13316 = DIRECTION ( 'NONE',  ( 0.2306359803922025109, 0.9730401042858035643, -5.112869192352692394E-15 ) ) ;
#13317 = LOCAL_TIME ( 14, 11, 27.00000000000000000, #5875 ) ;
#13318 = VECTOR ( 'NONE', #21693, 1000.000000000000000 ) ;
#13319 = EDGE_CURVE ( 'NONE', #10293, #23272, #5309, .T. ) ;
#13320 =( LENGTH_UNIT ( ) NAMED_UNIT ( * ) SI_UNIT ( .MILLI., .METRE. ) );
#13321 = VECTOR ( 'NONE', #18723, 1000.000000000000227 ) ;
#13322 = DIRECTION ( 'NONE',  ( 0.000000000000000000, -1.000000000000000000, 2.081668171172168119E-15 ) ) ;
#13323 = PERSON_AND_ORGANIZATION ( #11966, #8758 ) ;
#13324 = VERTEX_POINT ( 'NONE', #2096 ) ;
#13325 = DIRECTION ( 'NONE',  ( -0.1630842657209355673, -0.6880432561069612651, -0.7071067811865432429 ) ) ;
#13326 = ADVANCED_FACE ( 'NONE', ( #16571 ), #9052, .F. ) ;
#13327 = CARTESIAN_POINT ( 'NONE',  ( -20.00000000000190070, -20.00000000000000000, -8.499999999995459632 ) ) ;
#13328 = ORIENTED_EDGE ( 'NONE', *, *, #1127, .F. ) ;
#13329 = EDGE_CURVE ( 'NONE', #11391, #14490, #7346, .T. ) ;
#13330 = APPROVAL_PERSON_ORGANIZATION ( #16133, #11875, #14592 ) ;
#13331 = FACE_OUTER_BOUND ( 'NONE', #20260, .T. ) ;
#13332 = EDGE_CURVE ( 'NONE', #5825, #551, #3736, .T. ) ;
#13333 = CARTESIAN_POINT ( 'NONE',  ( 113.4570673249340018, -28.10438863268850085, -3.399999999999949729 ) ) ;
#13334 = LOCAL_TIME ( 14, 11, 27.00000000000000000, #7056 ) ;
#13335 = ORIENTED_EDGE ( 'NONE', *, *, #3818, .T. ) ;
#13336 = CYLINDRICAL_SURFACE ( 'NONE', #1592, 0.0009999999998218898900 ) ;
#13337 = VECTOR ( 'NONE', #15779, 1000.000000000000227 ) ;
#13338 = DATE_AND_TIME ( #500, #4577 ) ;
#13339 = ORIENTED_EDGE ( 'NONE', *, *, #17029, .F. ) ;
#13340 = ORIENTED_EDGE ( 'NONE', *, *, #16207, .F. ) ;
#13341 = DIRECTION ( 'NONE',  ( 2.269747459788994803E-13, 2.220446049250330436E-15, 1.000000000000000000 ) ) ;
#13342 = DIRECTION ( 'NONE',  ( 0.2306359803922076457, 0.9730401042858023430, 0.000000000000000000 ) ) ;
#13343 = CC_DESIGN_APPROVAL ( #23407, ( #8779 ) ) ;
#13344 = ORIENTED_EDGE ( 'NONE', *, *, #15363, .T. ) ;
#13345 = CALENDAR_DATE ( 2026, 31, 10 ) ;
#13346 = DIRECTION ( 'NONE',  ( 0.000000000000000000, -4.336808689942006376E-14, -1.000000000000000000 ) ) ;
#13347 = DIRECTION ( 'NONE',  ( 0.000000000000000000, 1.000000000000000000, -5.035481788031372371E-15 ) ) ;
#13348 = PERSON_AND_ORGANIZATION ( #6558, #14165 ) ;
#13349 = DIRECTION ( 'NONE',  ( 0.9730401042858035643, -0.2306359803922028717, -5.959266323858674978E-17 ) ) ;
#13350 = LOCAL_TIME ( 14, 11, 27.00000000000000000, #5293 ) ;
#13351 = CIRCLE ( 'NONE', #6139, 0.5000000000000004441 ) ;
#13352 = DIRECTION ( 'NONE',  ( -1.000000000000000000, 0.000000000000000000, 0.000000000000000000 ) ) ;
#13353 = CARTESIAN_POINT ( 'NONE',  ( 13.68761142428060040, 14.96724437631790039, -3.520083394366879149E-15 ) ) ;
#13354 = PERSON_AND_ORGANIZATION_ROLE ( 'creator' ) ;
#13355 = SECURITY_CLASSIFICATION ( '', '', #542 ) ;
#13356 = DIRECTION ( 'NONE',  ( 0.000000000000000000, 0.000000000000000000, -1.000000000000000000 ) ) ;
#13357 = LINE ( 'NONE', #15248, #4098 ) ;
#13358 = ADVANCED_FACE ( 'NONE', ( #5657 ), #20281, .T. ) ;
#13359 = CARTESIAN_POINT ( 'NONE',  ( -20.00000000397450250, 22.95208919256889857, -7.999999999995548450 ) ) ;
#13360 = CYLINDRICAL_SURFACE ( 'NONE', #21222, 12.50000000000000533 ) ;
#13361 = DIRECTION ( 'NONE',  ( -3.099353312215989243E-62, 9.554441540188157279E-93, 1.000000000000000000 ) ) ;
#13362 = CARTESIAN_POINT ( 'NONE',  ( 117.1241794131700118, -12.63305097454420078, -15.90000000000000036 ) ) ;
#13363 = ORIENTED_EDGE ( 'NONE', *, *, #19389, .T. ) ;
#13364 = APPROVAL_PERSON_ORGANIZATION ( #17618, #22560, #3346 ) ;
#13365 = EDGE_LOOP ( 'NONE', ( #21586, #8282 ) ) ;
#13366 = LINE ( 'NONE', #20482, #10371 ) ;
#13367 = CARTESIAN_POINT ( 'NONE',  ( -60.06514239919540188, -6.814592325618320068, 5.500000000000099476 ) ) ;
#13368 = ORIENTED_EDGE ( 'NONE', *, *, #17872, .T. ) ;
#13369 = AXIS2_PLACEMENT_3D ( 'NONE', #19605, #23151, #21390 ) ;
#13370 = VECTOR ( 'NONE', #10635, 1000.000000000000000 ) ;
#13371 = DIRECTION ( 'NONE',  ( 2.982858504489139758E-17, -2.441916418604790135E-15, -1.000000000000000000 ) ) ;
#13372 = ORIENTED_EDGE ( 'NONE', *, *, #10741, .T. ) ;
#13373 = AXIS2_PLACEMENT_3D ( 'NONE', #4835, #16112, #22991 ) ;
#13374 = VECTOR ( 'NONE', #18836, 1000.000000000000000 ) ;
#13375 = LINE ( 'NONE', #16815, #7979 ) ;
#13376 = LOCAL_TIME ( 14, 11, 27.00000000000000000, #10930 ) ;
#13377 = APPLICATION_PROTOCOL_DEFINITION ( 'international standard', 'config_control_design', 1994, #1824 ) ;
#13378 = CARTESIAN_POINT ( 'NONE',  ( 37.02539408398538257, 11.29029616550548454, -8.817835639223822852 ) ) ;
#13379 = VECTOR ( 'NONE', #3104, 1000.000000000000000 ) ;
#13380 = DIRECTION ( 'NONE',  ( 0.000000000000000000, 0.000000000000000000, 1.000000000000000000 ) ) ;
#13381 = AXIS2_PLACEMENT_3D ( 'NONE', #11534, #16955, #3900 ) ;
#13382 = CARTESIAN_POINT ( 'NONE',  ( 34.88044566782589584, 28.44271146055899990, 17.99999999999970157 ) ) ;
#13383 = ORIENTED_EDGE ( 'NONE', *, *, #22820, .F. ) ;
#13384 = LOCAL_TIME ( 14, 11, 27.00000000000000000, #2115 ) ;
#13385 = DIRECTION ( 'NONE',  ( -0.2306359803922028995, -0.9730401042858036753, 1.343075398093749487E-16 ) ) ;
#13386 = CIRCLE ( 'NONE', #8480, 4.250000000000000000 ) ;
#13387 = EDGE_LOOP ( 'NONE', ( #16106, #13453, #4419, #12128 ) ) ;
#13388 = CARTESIAN_POINT ( 'NONE',  ( -62.94230935805129690, 13.36384453327990052, -5.515482965309170069E-15 ) ) ;
#13389 = AXIS2_PLACEMENT_3D ( 'NONE', #5264, #12525, #3959 ) ;
#13390 = AXIS2_PLACEMENT_3D ( 'NONE', #14064, #8378, #19299 ) ;
#13391 = DIRECTION ( 'NONE',  ( 1.000000000000000000, 0.000000000000000000, 0.000000000000000000 ) ) ;
#13392 = ORIENTED_EDGE ( 'NONE', *, *, #3160, .T. ) ;
#13393 = CARTESIAN_POINT ( 'NONE',  ( 34.85554549375144973, 7.839538622613233976, -8.762651562745512379 ) ) ;
#13394 = DIRECTION ( 'NONE',  ( -0.005235963827063078342, 0.9999862922474496152, 2.538287662677322384E-14 ) ) ;
#13395 = EDGE_LOOP ( 'NONE', ( #19491, #8125, #12013, #21904 ) ) ;
#13396 = UNCERTAINTY_MEASURE_WITH_UNIT (LENGTH_MEASURE( 1.000000000000000082E-05 ), #9824, 'distance_accuracy_value', 'NONE');
#13397 = APPROVAL_DATE_TIME ( #907, #6897 ) ;
#13398 = CARTESIAN_POINT ( 'NONE',  ( 43.45766680872420551, 21.27115113520920175, -13.00000000000000000 ) ) ;
#13399 = AXIS2_PLACEMENT_3D ( 'NONE', #5060, #12324, #3029 ) ;
#13400 = EDGE_LOOP ( 'NONE', ( #15674, #14383, #8666, #16506 ) ) ;
#13401 = ADVANCED_FACE ( 'NONE', ( #23467 ), #12908, .T. ) ;
#13402 = AXIS2_PLACEMENT_3D ( 'NONE', #17079, #9630, #9984 ) ;
#13403 = CALENDAR_DATE ( 2026, 31, 10 ) ;
#13404 = DIRECTION ( 'NONE',  ( -2.656137997592320068E-16, 6.783012436524469908E-17, 1.000000000000000000 ) ) ;
#13405 = ADVANCED_FACE ( 'NONE', ( #3648 ), #1856, .F. ) ;
#13406 = LOCAL_TIME ( 14, 11, 27.00000000000000000, #7185 ) ;
#13407 = EDGE_LOOP ( 'NONE', ( #20989, #7601, #8163, #1264 ) ) ;
#13408 = ORIENTED_EDGE ( 'NONE', *, *, #8870, .T. ) ;
#13409 = COORDINATED_UNIVERSAL_TIME_OFFSET ( 0, 0, .AHEAD. ) ;
#13410 = AXIS2_PLACEMENT_3D ( 'NONE', #7178, #3829, #12650 ) ;
#13411 = CALENDAR_DATE ( 2026, 31, 10 ) ;
#13412 =( BOUNDED_CURVE ( )  B_SPLINE_CURVE ( 2, ( #10376, #4529, #8218 ),
 .UNSPECIFIED., .F., .T. ) 
 B_SPLINE_CURVE_WITH_KNOTS ( ( 3, 3 ),
 ( 0.000000000000000000, 0.1168436138077924430 ),
 .UNSPECIFIED. ) 
 CURVE ( )  GEOMETRIC_REPRESENTATION_ITEM ( )  RATIONAL_B_SPLINE_CURVE ( ( 1.000000000000000000, 1.077350269189624621, 1.077350269189625065 ) ) 
 REPRESENTATION_ITEM ( '' )  );
#13413 = CYLINDRICAL_SURFACE ( 'NONE', #568, 12.49999999999999645 ) ;
#13414 = EDGE_CURVE ( 'NONE', #8216, #21157, #8636, .T. ) ;
#13415 = EDGE_CURVE ( 'NONE', #21187, #1005, #11270, .T. ) ;
#13417 = VECTOR ( 'NONE', #2503, 1000.000000000000000 ) ;
#13416 = CARTESIAN_POINT ( 'NONE',  ( -22.49917142882856069, 22.89791325974001879, 2.499999999999900524 ) ) ;
#13418 = VERTEX_POINT ( 'NONE', #2213 ) ;
#13419 = PERSON_AND_ORGANIZATION ( #11966, #8758 ) ;
#13420 = CONICAL_SURFACE ( 'NONE', #21378, 2.624999999999998668, 0.4636476090008128104 ) ;
#13421 = ORIENTED_EDGE ( 'NONE', *, *, #6741, .T. ) ;
#13422 = VECTOR ( 'NONE', #2874, 999.9999999999998863 ) ;
#13423 = DIRECTION ( 'NONE',  ( 1.138590270679730064E-14, 2.220446049251240387E-15, 1.000000000000000000 ) ) ;
#13424 = DIRECTION ( 'NONE',  ( 0.000000000000000000, 0.000000000000000000, 1.000000000000000000 ) ) ;
#13425 = EDGE_LOOP ( 'NONE', ( #13278, #15914, #21923, #9042, #18392, #16859 ) ) ;
#13426 = DIRECTION ( 'NONE',  ( 1.000000000000000000, 3.210834492181040124E-17, 1.751623080406019734E-47 ) ) ;
#13427 = AXIS2_PLACEMENT_3D ( 'NONE', #12918, #11284, #16583 ) ;
#13428 = DIRECTION ( 'NONE',  ( -2.982858504577319616E-17, 2.441916418604790135E-15, 1.000000000000000000 ) ) ;
#13429 = DIRECTION ( 'NONE',  ( -6.662111519016958720E-09, 1.000000000000000000, -2.523234146875356491E-15 ) ) ;
#13430 = ORIENTED_EDGE ( 'NONE', *, *, #11185, .T. ) ;
#13431 = VERTEX_POINT ( 'NONE', #4362 ) ;
#13432 = CARTESIAN_POINT ( 'NONE',  ( 30.50389457288209982, -2.378844316418729843, 13.00000000000000000 ) ) ;
#13433 = ORIENTED_EDGE ( 'NONE', *, *, #6919, .F. ) ;
#13434 = CALENDAR_DATE ( 2026, 31, 10 ) ;
#13435 = EDGE_CURVE ( 'NONE', #23272, #23261, #20734, .T. ) ;
#13436 = ORIENTED_EDGE ( 'NONE', *, *, #9186, .T. ) ;
#13437 = VERTEX_POINT ( 'NONE', #6134 ) ;
#13438 = DIRECTION ( 'NONE',  ( 3.099353312215989243E-62, -1.403547063447849893E-77, -1.000000000000000000 ) ) ;
#13439 = CALENDAR_DATE ( 2026, 31, 10 ) ;
#13440 = CARTESIAN_POINT ( 'NONE',  ( -19.99999998251385946, -22.50000000000000000, -7.999999999995453415 ) ) ;
#13441 = CC_DESIGN_PERSON_AND_ORGANIZATION_ASSIGNMENT ( #17268, #1087, ( #3753 ) ) ;
#13442 = CIRCLE ( 'NONE', #12680, 6.500000000000000000 ) ;
#13443 = APPROVAL ( #9875, 'UNSPECIFIED' ) ;
#13444 = DIRECTION ( 'NONE',  ( -0.9997648975362233292, -0.02168293463497958373, 0.000000000000000000 ) ) ;
#13445 = CIRCLE ( 'NONE', #11176, 2.500000000000000888 ) ;
#13446 = EDGE_CURVE ( 'NONE', #7239, #7334, #901, .T. ) ;
#13447 = ADVANCED_FACE ( 'NONE', ( #2463 ), #9600, .F. ) ;
#13448 = DIRECTION ( 'NONE',  ( 0.9730401042858035643, -0.2306359803922028717, -5.432877459303547053E-17 ) ) ;
#13449 = CALENDAR_DATE ( 2026, 31, 10 ) ;
#13450 = VERTEX_POINT ( 'NONE', #9953 ) ;
#13451 = CARTESIAN_POINT ( 'NONE',  ( -20.00000000000000000, -20.00000000000000000, -2.500000000000000000 ) ) ;
#13452 = LINE ( 'NONE', #15101, #1761 ) ;
#13453 = ORIENTED_EDGE ( 'NONE', *, *, #12971, .T. ) ;
#13454 = CARTESIAN_POINT ( 'NONE',  ( 114.1489752661110089, -25.18526831983100323, 3.399999999999999911 ) ) ;
#13455 = CARTESIAN_POINT ( 'NONE',  ( -65.82123935389580538, 11.86253283145240012, -5.000000000000000000 ) ) ;
#13456 = VERTEX_POINT ( 'NONE', #17185 ) ;
#13457 = FACE_BOUND ( 'NONE', #661, .T. ) ;
#13458 = APPLICATION_PROTOCOL_DEFINITION ( 'international standard', 'config_control_design', 1994, #10360 ) ;
#13459 = EDGE_CURVE ( 'NONE', #8556, #20891, #20424, .T. ) ;
#13460 = ORIENTED_EDGE ( 'NONE', *, *, #5192, .T. ) ;
#13461 = ORIENTED_EDGE ( 'NONE', *, *, #6252, .T. ) ;
#13462 = CARTESIAN_POINT ( 'NONE',  ( -20.00000000397360012, 22.95208919256889857, -5.000000000000000000 ) ) ;
#13463 = LINE ( 'NONE', #20695, #14767 ) ;
#13464 = ORIENTED_EDGE ( 'NONE', *, *, #17073, .F. ) ;
#13465 = APPLICATION_PROTOCOL_DEFINITION ( 'international standard', 'config_control_design', 1994, #22188 ) ;
#13466 = FACE_BOUND ( 'NONE', #14631, .T. ) ;
#13467 = CC_DESIGN_DATE_AND_TIME_ASSIGNMENT ( #13281, #22176, ( #17927 ) ) ;
#13468 = PRODUCT_DEFINITION ( 'UNKNOWN', '', #23156, #21325 ) ;
#13469 = FACE_OUTER_BOUND ( 'NONE', #15611, .T. ) ;
#13470 = CALENDAR_DATE ( 2026, 31, 10 ) ;
#13471 = FACE_OUTER_BOUND ( 'NONE', #17686, .T. ) ;
#13472 = EDGE_CURVE ( 'NONE', #11832, #16045, #18500, .T. ) ;
#13473 = EDGE_CURVE ( 'NONE', #2977, #21983, #18857, .T. ) ;
#13474 = CARTESIAN_POINT ( 'NONE',  ( 31.11077410011089839, -1.335996977273280262, -15.00000000000039968 ) ) ;
#13475 = DATE_AND_TIME ( #15833, #12219 ) ;
#13476 = CARTESIAN_POINT ( 'NONE',  ( -62.75803838139569280, -21.82899804532949872, -5.536374493610579731E-15 ) ) ;
#13477 = LINE ( 'NONE', #22133, #15474 ) ;
#13478 = FACE_BOUND ( 'NONE', #23332, .T. ) ;
#13479 = CARTESIAN_POINT ( 'NONE',  ( 66.60056952104010008, 2.425487965306460048, 1.173314102775059961E-14 ) ) ;
#13480 = CARTESIAN_POINT ( 'NONE',  ( -3.458317987535630689, 19.03127855354509990, 4.999999999999999112 ) ) ;
#13481 = ORIENTED_EDGE ( 'NONE', *, *, #22183, .T. ) ;
#13482 = EDGE_CURVE ( 'NONE', #22277, #5211, #7918, .T. ) ;
#13483 = CIRCLE ( 'NONE', #10839, 9.000000000000003553 ) ;
#13484 = EDGE_LOOP ( 'NONE', ( #2252, #13038 ) ) ;
#13485 = CARTESIAN_POINT ( 'NONE',  ( 3.061616997868383141E-16, -2.500000000000000444, -2.500000000000000000 ) ) ;
#13486 = DIRECTION ( 'NONE',  ( -6.123230174520380038E-17, -4.962644601432250805E-15, -1.000000000000000000 ) ) ;
#13487 = ORIENTED_EDGE ( 'NONE', *, *, #23264, .T. ) ;
#13488 = DIRECTION ( 'NONE',  ( 3.210834492194349687E-17, -2.441916418604790135E-15, -1.000000000000000000 ) ) ;
#13489 = ORIENTED_EDGE ( 'NONE', *, *, #4849, .T. ) ;
#13490 = DIRECTION ( 'NONE',  ( -0.002617981913558647261, 0.4999931461237237529, 0.8660254037844391517 ) ) ;
#13491 = DATE_AND_TIME ( #22511, #7339 ) ;
#13492 = CARTESIAN_POINT ( 'NONE',  ( -60.05196788195259927, 12.68574396146170180, 5.000000000000000000 ) ) ;
#13493 = EDGE_CURVE ( 'NONE', #21983, #21398, #15040, .T. ) ;
#13494 = PRODUCT_DEFINITION_SHAPE ( 'NONE', 'NONE',  #9377 ) ;
#13495 = EDGE_CURVE ( 'NONE', #21501, #638, #22622, .T. ) ;
#13496 = SECURITY_CLASSIFICATION_LEVEL ( 'unclassified' ) ;
#13497 =( NAMED_UNIT ( * ) SI_UNIT ( $, .STERADIAN. ) SOLID_ANGLE_UNIT ( ) );
#13498 = CARTESIAN_POINT ( 'NONE',  ( -20.00000000000000000, -20.00000000000000000, 0.000000000000000000 ) ) ;
#13499 = CARTESIAN_POINT ( 'NONE',  ( -26.75617730459320143, 6.359992804688680224, 2.500000000000090150 ) ) ;
#13500 = ORIENTED_EDGE ( 'NONE', *, *, #5639, .T. ) ;
#13501 = CARTESIAN_POINT ( 'NONE',  ( -29.01760921662840076, 6.974057232812999274, -3.750000000000000000 ) ) ;
#13502 = AXIS2_PLACEMENT_3D ( 'NONE', #97, #19943, #14597 ) ;
#13503 = LINE ( 'NONE', #7808, #11049 ) ;
#13504 = ORIENTED_EDGE ( 'NONE', *, *, #16938, .T. ) ;
#13505 = DIRECTION ( 'NONE',  ( 0.2306359803922080620, 0.9730401042858023430, 5.907067092757398303E-15 ) ) ;
#13506 = DIRECTION ( 'NONE',  ( -0.9997648976141043642, -0.02168293104402130300, 0.000000000000000000 ) ) ;
#13507 = PERSON_AND_ORGANIZATION ( #4259, #15643 ) ;
#13508 = DIRECTION ( 'NONE',  ( -0.9730401042858024541, 0.2306359803922080898, 5.959266323858942451E-17 ) ) ;
#13509 = EDGE_LOOP ( 'NONE', ( #3040, #18979, #12611, #1402 ) ) ;
#13510 = CC_DESIGN_PERSON_AND_ORGANIZATION_ASSIGNMENT ( #22356, #9692, ( #8384 ) ) ;
#13511 = CALENDAR_DATE ( 2026, 31, 10 ) ;
#13512 = FACE_OUTER_BOUND ( 'NONE', #14841, .T. ) ;
#13513 = ORIENTED_EDGE ( 'NONE', *, *, #17234, .F. ) ;
#13514 =( GEOMETRIC_REPRESENTATION_CONTEXT ( 3 ) GLOBAL_UNCERTAINTY_ASSIGNED_CONTEXT ( ( #7293 ) ) GLOBAL_UNIT_ASSIGNED_CONTEXT ( ( #20115, #5870, #9315 ) ) REPRESENTATION_CONTEXT ( 'NONE', 'WORKASPACE' ) );
#13515 = VERTEX_POINT ( 'NONE', #4235 ) ;
#13516 = APPROVAL_DATE_TIME ( #790, #14898 ) ;
#13517 = AXIS2_PLACEMENT_3D ( 'NONE', #2391, #21030, #1058 ) ;
#13518 = DIRECTION ( 'NONE',  ( 1.239096229992445915E-15, 4.969341027244109908E-15, 1.000000000000000000 ) ) ;
#13519 = CARTESIAN_POINT ( 'NONE',  ( 35.09747506357100377, 11.43410645592859964, 29.25000000000000000 ) ) ;
#13520 = ORIENTED_EDGE ( 'NONE', *, *, #13032, .T. ) ;
#13521 = APPLICATION_CONTEXT ( 'configuration controlled 3d designs of mechanical parts and assemblies' ) ;
#13522 = EDGE_CURVE ( 'NONE', #11347, #8547, #11706, .T. ) ;
#13523 = DATE_TIME_ROLE ( 'classification_date' ) ;
#13524 = CIRCLE ( 'NONE', #23359, 3.499999999999999556 ) ;
#13525 = ORIENTED_EDGE ( 'NONE', *, *, #20853, .T. ) ;
#13526 = DIRECTION ( 'NONE',  ( -0.9730401042858036753, 0.2306359803922031493, 5.432877459303543355E-17 ) ) ;
#13527 = DIRECTION ( 'NONE',  ( -0.9730401042858035643, 0.2306359803922028717, 5.667427308550587516E-17 ) ) ;
#13528 = ORIENTED_EDGE ( 'NONE', *, *, #15619, .T. ) ;
#13529 = CARTESIAN_POINT ( 'NONE',  ( -19.49999999982519938, -0.1021026942257719922, 2.500000000000000000 ) ) ;
#13530 = DIRECTION ( 'NONE',  ( -2.829953705592110306E-16, -9.355573283744330345E-16, -1.000000000000000000 ) ) ;
#13531 = FACE_OUTER_BOUND ( 'NONE', #3977, .T. ) ;
#13532 = VERTEX_POINT ( 'NONE', #9722 ) ;
#13533 = EDGE_LOOP ( 'NONE', ( #3338, #23128 ) ) ;
#13534 = CARTESIAN_POINT ( 'NONE',  ( -26.75617730459320143, 6.359992804688680224, -2.500000000000090150 ) ) ;
#13535 = VERTEX_POINT ( 'NONE', #16936 ) ;
#13536 = MECHANICAL_CONTEXT ( 'NONE', #15179, 'mechanical' ) ;
#13537 = EDGE_LOOP ( 'NONE', ( #21843, #7258, #17205, #14000 ) ) ;
#13538 = ORIENTED_EDGE ( 'NONE', *, *, #9731, .T. ) ;
#13539 = LINE ( 'NONE', #20783, #13417 ) ;
#13540 = SHAPE_REPRESENTATION ( '1602p_c_15', ( #12739 ), #3642 ) ;
#13541 = CIRCLE ( 'NONE', #14684, 2.066999999999999726 ) ;
#13542 = PERSON_AND_ORGANIZATION ( #11966, #8758 ) ;
#13543 = CIRCLE ( 'NONE', #12787, 2.500000000000000888 ) ;
#13544 = DIRECTION ( 'NONE',  ( 0.9730401042858035643, -0.2306359803922028717, -5.959266323858667582E-17 ) ) ;
#13545 = VECTOR ( 'NONE', #8491, 1000.000000000000000 ) ;
#13546 = VECTOR ( 'NONE', #16429, 999.9999999999998863 ) ;
#13547 = DIRECTION ( 'NONE',  ( -0.6660003063074659835, 0.7459514675891198987, 0.000000000000000000 ) ) ;
#13548 = ADVANCED_FACE ( 'NONE', ( #662 ), #4082, .T. ) ;
#13549 = PERSON_AND_ORGANIZATION_ROLE ( 'creator' ) ;
#13550 = ORIENTED_EDGE ( 'NONE', *, *, #465, .T. ) ;
#13551 = AXIS2_PLACEMENT_3D ( 'NONE', #13912, #19153, #15451 ) ;
#13552 = CARTESIAN_POINT ( 'NONE',  ( -25.00842861987479893, -15.87143667223269894, 23.00000000000000000 ) ) ;
#13553 = DIRECTION ( 'NONE',  ( -1.000000000000000000, 2.270069654138870255E-15, -3.099353312215989243E-62 ) ) ;
#13554 = ORIENTED_EDGE ( 'NONE', *, *, #16902, .F. ) ;
#13555 = CC_DESIGN_DATE_AND_TIME_ASSIGNMENT ( #22526, #4370, ( #17915 ) ) ;
#13556 = AXIS2_PLACEMENT_3D ( 'NONE', #4589, #22741, #10433 ) ;
#13557 = CARTESIAN_POINT ( 'NONE',  ( -59.87132660632070014, -21.81388311970430038, -5.000000000000000000 ) ) ;
#13558 = CIRCLE ( 'NONE', #15065, 2.009240000000000137 ) ;
#13559 = CYLINDRICAL_SURFACE ( 'NONE', #8832, 2.500000000000000000 ) ;
#13560 = VERTEX_POINT ( 'NONE', #20631 ) ;
#13561 = CARTESIAN_POINT ( 'NONE',  ( 111.8137341348020044, 5.068973512656589797, 13.00000000000000000 ) ) ;
#13562 = EDGE_CURVE ( 'NONE', #11869, #13768, #13151, .T. ) ;
#13563 = EDGE_CURVE ( 'NONE', #13022, #1396, #768, .T. ) ;
#13564 = PERSON_AND_ORGANIZATION ( #11966, #8758 ) ;
#13565 = EDGE_LOOP ( 'NONE', ( #19853, #22428, #3824, #18678 ) ) ;
#13566 = ORIENTED_EDGE ( 'NONE', *, *, #22139, .F. ) ;
#13567 = CARTESIAN_POINT ( 'NONE',  ( -20.00000000000000000, -20.00000000000000000, 5.000000000000000000 ) ) ;
#13568 = DIRECTION ( 'NONE',  ( 0.8846153846153640421, -0.4663213712685829182, 0.000000000000000000 ) ) ;
#13569 = ORIENTED_EDGE ( 'NONE', *, *, #1383, .T. ) ;
#13570 = VECTOR ( 'NONE', #2940, 1000.000000000000114 ) ;
#13571 = COORDINATED_UNIVERSAL_TIME_OFFSET ( 0, 0, .AHEAD. ) ;
#13572 = DIRECTION ( 'NONE',  ( 0.9730401042858024541, -0.2306359803922080898, -5.959266323863172718E-17 ) ) ;
#13573 = DIRECTION ( 'NONE',  ( 0.000000000000000000, 0.000000000000000000, -1.000000000000000000 ) ) ;
#13574 = TOROIDAL_SURFACE ( 'NONE', #9032, 2.600000000000000089, 0.1000000000000000056 ) ;
#13575 = CALENDAR_DATE ( 2026, 31, 10 ) ;
#13576 = FACE_OUTER_BOUND ( 'NONE', #8747, .T. ) ;
#13577 = AXIS2_PLACEMENT_3D ( 'NONE', #1210, #19173, #17272 ) ;
#13578 = SHAPE_REPRESENTATION_RELATIONSHIP ( 'NONE' , 'NONE' ,  #16866, #12780 ) ;
#13579 = DIRECTION ( 'NONE',  ( -2.269747459788999852E-13, -2.220446049250320181E-15, -1.000000000000000000 ) ) ;
#13580 = EDGE_CURVE ( 'NONE', #2399, #2378, #6258, .T. ) ;
#13581 = CALENDAR_DATE ( 2026, 31, 10 ) ;
#13582 = CARTESIAN_POINT ( 'NONE',  ( 37.46113131852679601, -4.027891576221660053, 13.00000000000000000 ) ) ;
#13583 = CARTESIAN_POINT ( 'NONE',  ( 35.59419854219520118, 9.774809681453550780, 26.88000000000000256 ) ) ;
#13584 = CC_DESIGN_PERSON_AND_ORGANIZATION_ASSIGNMENT ( #22729, #6722, ( #17082 ) ) ;
#13585 = EDGE_CURVE ( 'NONE', #17568, #4807, #1425, .T. ) ;
#13586 = PLANE ( 'NONE',  #18471 ) ;
#13587 = DIRECTION ( 'NONE',  ( -0.6880432561069586006, 0.1630842657209346236, 0.7071067811865459074 ) ) ;
#13588 = CC_DESIGN_PERSON_AND_ORGANIZATION_ASSIGNMENT ( #8908, #19407, ( #11960 ) ) ;
#13589 = LINE ( 'NONE', #20038, #14499 ) ;
#13590 = DIRECTION ( 'NONE',  ( -0.9286452767786568252, -1.871119812896369614E-17, -0.3709689338970204586 ) ) ;
#13591 = EDGE_CURVE ( 'NONE', #22023, #8287, #17304, .T. ) ;
#13593 = ORIENTED_EDGE ( 'NONE', *, *, #11641, .T. ) ;
#13592 = ADVANCED_FACE ( 'NONE', ( #17768 ), #11979, .T. ) ;
#13594 = CC_DESIGN_PERSON_AND_ORGANIZATION_ASSIGNMENT ( #17218, #22422, ( #19033 ) ) ;
#13595 = VERTEX_POINT ( 'NONE', #15862 ) ;
#13596 = FACE_OUTER_BOUND ( 'NONE', #19183, .T. ) ;
#13597 = VECTOR ( 'NONE', #10046, 1000.000000000000000 ) ;
#13598 = DIRECTION ( 'NONE',  ( 0.7071067811865476838, -1.387778780781444689E-15, 0.7071067811865473507 ) ) ;
#13599 = EDGE_LOOP ( 'NONE', ( #3581, #2516 ) ) ;
#13600 = CARTESIAN_POINT ( 'NONE',  ( 37.56481403710121469, 24.44795204016919854, 12.00000000000000000 ) ) ;
#13601 = VERTEX_POINT ( 'NONE', #19199 ) ;
#13602 = CARTESIAN_POINT ( 'NONE',  ( -20.00000000000000000, -20.00000000000000000, -5.499999999995469402 ) ) ;
#13603 = COORDINATED_UNIVERSAL_TIME_OFFSET ( 0, 0, .AHEAD. ) ;
#13604 = DIRECTION ( 'NONE',  ( -0.2306359803922066187, -0.9730401042858026761, 0.000000000000000000 ) ) ;
#13605 = SECURITY_CLASSIFICATION_LEVEL ( 'unclassified' ) ;
#13606 = CARTESIAN_POINT ( 'NONE',  ( 0.000000000000000000, 0.000000000000000000, 0.000000000000000000 ) ) ;
#13607 = CARTESIAN_POINT ( 'NONE',  ( -2.291879384893320104, 10.94490600546980019, 2.500000000000000000 ) ) ;
#13608 = CARTESIAN_POINT ( 'NONE',  ( -62.73971250800079957, -25.32895006819559924, 5.000000000000000000 ) ) ;
#13609 = ADVANCED_FACE ( 'NONE', ( #19428 ), #13855, .T. ) ;
#13610 = CLOSED_SHELL ( 'NONE', ( #6770, #5695, #16503, #12543, #11303, #17746, #4422, #4475, #1975, #17106, #14728, #22827, #18265, #21, #9661 ) ) ;
#13611 = AXIS2_PLACEMENT_3D ( 'NONE', #1982, #21684, #16238 ) ;
#13612 = CARTESIAN_POINT ( 'NONE',  ( 41.15130700480209924, 11.54075009235119964, -15.90000000000000036 ) ) ;
#13613 = VERTEX_POINT ( 'NONE', #3273 ) ;
#13614 = CARTESIAN_POINT ( 'NONE',  ( 37.14513723987899851, -6.299761344113198547, 13.00000000000000000 ) ) ;
#13615 = ADVANCED_BREP_SHAPE_REPRESENTATION ( '', ( #17052, #12739 ), #1341 ) ;
#13616 = ADVANCED_FACE ( 'NONE', ( #6848 ), #3037, .T. ) ;
#13617 = DIRECTION ( 'NONE',  ( 1.000000000000000000, -1.466984912809929871E-16, -5.345529420184390105E-52 ) ) ;
#13618 = ORIENTED_EDGE ( 'NONE', *, *, #4421, .T. ) ;
#13619 = CARTESIAN_POINT ( 'NONE',  ( 105.3404740731333078, -22.24134309433305390, 13.00000000000000000 ) ) ;
#13620 = VECTOR ( 'NONE', #20138, 1000.000000000000114 ) ;
#13621 = LINE ( 'NONE', #22393, #19392 ) ;
#13622 = ADVANCED_FACE ( 'NONE', ( #17535 ), #3319, .F. ) ;
#13623 = DATE_AND_TIME ( #8166, #7254 ) ;
#13624 = EDGE_CURVE ( 'NONE', #2339, #7183, #2925, .T. ) ;
#13625 = DIRECTION ( 'NONE',  ( -0.2306359803922076457, -0.9730401042858025651, 0.000000000000000000 ) ) ;
#13626 = ORIENTED_EDGE ( 'NONE', *, *, #6936, .F. ) ;
#13627 = VERTEX_POINT ( 'NONE', #14082 ) ;
#13628 = PERSON_AND_ORGANIZATION ( #11966, #8758 ) ;
#13629 = CARTESIAN_POINT ( 'NONE',  ( -16.20883170868506085, 30.27513909371458567, -4.938659382458227626E-15 ) ) ;
#13630 = VERTEX_POINT ( 'NONE', #5067 ) ;
#13631 = CARTESIAN_POINT ( 'NONE',  ( -21.99996573044222004, -0.1151926037937907599, 2.500000000000000444 ) ) ;
#13632 = DATE_AND_TIME ( #17432, #15274 ) ;
#13633 = PRODUCT_DEFINITION_SHAPE ( 'NONE', 'NONE',  #19552 ) ;
#13634 = DIRECTION ( 'NONE',  ( 5.039851780001396616E-28, 2.220446049301850153E-15, 1.000000000000000000 ) ) ;
#13635 = CC_DESIGN_APPROVAL ( #8513, ( #3753 ) ) ;
#13636 = AXIS2_PLACEMENT_3D ( 'NONE', #17131, #4191, #18699 ) ;
#13637 = CYLINDRICAL_SURFACE ( 'NONE', #22493, 4.999999999999996447 ) ;
#13638 = EDGE_LOOP ( 'NONE', ( #5408, #969 ) ) ;
#13639 = PERSON_AND_ORGANIZATION ( #11966, #8758 ) ;
#13640 = ORIENTED_EDGE ( 'NONE', *, *, #11145, .T. ) ;
#13641 = EDGE_CURVE ( 'NONE', #6915, #5066, #10194, .T. ) ;
#13642 = FACE_OUTER_BOUND ( 'NONE', #12192, .T. ) ;
#13643 = DIRECTION ( 'NONE',  ( -2.347220324585850163E-14, -9.876950852243829821E-14, -1.000000000000000000 ) ) ;
#13644 = ORIENTED_EDGE ( 'NONE', *, *, #833, .F. ) ;
#13645 = DIRECTION ( 'NONE',  ( 1.138590270679734009E-14, 2.220446049251240387E-15, 1.000000000000000000 ) ) ;
#13646 = CYLINDRICAL_SURFACE ( 'NONE', #19125, 2.499999999999998668 ) ;
#13647 = CARTESIAN_POINT ( 'NONE',  ( -24.86147400983239919, -14.96352599016710094, -2.500000000000000000 ) ) ;
#13648 = VERTEX_POINT ( 'NONE', #6622 ) ;
#13649 = AXIS2_PLACEMENT_3D ( 'NONE', #830, #4407, #15559 ) ;
#13650 = ORIENTED_EDGE ( 'NONE', *, *, #15918, .T. ) ;
#13652 = AXIS2_PLACEMENT_3D ( 'NONE', #586, #4282, #6054 ) ;
#13651 = DIRECTION ( 'NONE',  ( 0.8846153846154072298, -0.4663213712685009837, 0.000000000000000000 ) ) ;
#13653 = ORIENTED_EDGE ( 'NONE', *, *, #8181, .T. ) ;
#13654 = SECURITY_CLASSIFICATION_LEVEL ( 'unclassified' ) ;
#13655 = VERTEX_POINT ( 'NONE', #8278 ) ;
#13656 = ORIENTED_EDGE ( 'NONE', *, *, #10435, .T. ) ;
#13657 = FACE_OUTER_BOUND ( 'NONE', #13407, .T. ) ;
#13658 = COORDINATED_UNIVERSAL_TIME_OFFSET ( 0, 0, .AHEAD. ) ;
#13659 = VECTOR ( 'NONE', #3598, 1000.000000000000114 ) ;
#13660 = EDGE_CURVE ( 'NONE', #1775, #9763, #9796, .T. ) ;
#13661 = CARTESIAN_POINT ( 'NONE',  ( 44.35571774535060996, 23.18255965125822371, -13.00000000000000000 ) ) ;
#13662 = CC_DESIGN_APPROVAL ( #22338, ( #7231 ) ) ;
#13663 = CARTESIAN_POINT ( 'NONE',  ( 0.000000000000000000, 0.000000000000000000, 0.000000000000000000 ) ) ;
#13664 = AXIS2_PLACEMENT_3D ( 'NONE', #22735, #11976, #1245 ) ;
#13665 = VECTOR ( 'NONE', #8722, 1000.000000000000114 ) ;
#13666 = DIRECTION ( 'NONE',  ( 0.000000000000000000, 0.000000000000000000, 1.000000000000000000 ) ) ;
#13667 = MECHANICAL_CONTEXT ( 'NONE', #15946, 'mechanical' ) ;
#13668 = ORIENTED_EDGE ( 'NONE', *, *, #21382, .T. ) ;
#13669 = DIRECTION ( 'NONE',  ( -6.123237831918669245E-17, 0.000000000000000000, 1.000000000000000000 ) ) ;
#13670 = PLANE ( 'NONE',  #16963 ) ;
#13671 = AXIS2_PLACEMENT_3D ( 'NONE', #550, #13265, #11632 ) ;
#13672 = ORIENTED_EDGE ( 'NONE', *, *, #7445, .T. ) ;
#13673 = DIRECTION ( 'NONE',  ( 0.000000000000000000, 1.000000000000000000, 0.000000000000000000 ) ) ;
#13674 = CARTESIAN_POINT ( 'NONE',  ( 5.000000000000000000, -28.60000000000000142, -6.250000000000000000 ) ) ;
#13675 = AXIS2_PLACEMENT_3D ( 'NONE', #6332, #17734, #19867 ) ;
#13676 = ORIENTED_EDGE ( 'NONE', *, *, #13015, .F. ) ;
#13677 = CARTESIAN_POINT ( 'NONE',  ( -25.00842861987479893, -15.87143667223269894, -23.00000000000000000 ) ) ;
#13678 = PERSON_AND_ORGANIZATION ( #11966, #8758 ) ;
#13679 = PRODUCT_DEFINITION_SHAPE ( 'NONE', 'NONE',  #9078 ) ;
#13680 = CC_DESIGN_APPROVAL ( #1247, ( #3714 ) ) ;
#13681 = EDGE_LOOP ( 'NONE', ( #16537, #8053, #21951, #6599 ) ) ;
#13682 = ORIENTED_EDGE ( 'NONE', *, *, #6286, .F. ) ;
#13683 = CARTESIAN_POINT ( 'NONE',  ( -19.49999999982379961, -0.1021026942259700004, -8.658030917271079259E-14 ) ) ;
#13684 = CARTESIAN_POINT ( 'NONE',  ( -62.93889088200999282, 12.71096966728388722, 4.999999999999999112 ) ) ;
#13685 = APPROVAL_PERSON_ORGANIZATION ( #21383, #4067, #5226 ) ;
#13686 = ORIENTED_EDGE ( 'NONE', *, *, #9288, .F. ) ;
#13687 = DATE_AND_TIME ( #970, #4989 ) ;
#13688 = ADVANCED_FACE ( 'NONE', ( #6486 ), #12209, .T. ) ;
#13689 = CARTESIAN_POINT ( 'NONE',  ( -20.00000000397270128, 22.95208919256889857, -4.999999999995559996 ) ) ;
#13690 = EDGE_CURVE ( 'NONE', #10034, #10146, #4461, .T. ) ;
#13691 = DIRECTION ( 'NONE',  ( 0.000000000000000000, 0.000000000000000000, -1.000000000000000000 ) ) ;
#13692 = PERSON_AND_ORGANIZATION_ROLE ( 'classification_officer' ) ;
#13693 = CARTESIAN_POINT ( 'NONE',  ( 120.8143550994449953, 2.935590694028619829, -13.00000000000000000 ) ) ;
#13694 = CIRCLE ( 'NONE', #13671, 2.500000000000000444 ) ;
#13695 = APPROVAL ( #8532, 'UNKNOWN' ) ;
#13696 = ADVANCED_FACE ( 'NONE', ( #17418 ), #8525, .F. ) ;
#13697 = EDGE_CURVE ( 'NONE', #10083, #21956, #15448, .T. ) ;
#13698 = DIRECTION ( 'NONE',  ( 6.123230199561449365E-17, 4.868008300101910084E-15, 1.000000000000000000 ) ) ;
#13699 = APPROVAL_ROLE ( '' ) ;
#13700 = CC_DESIGN_APPROVAL ( #6932, ( #19247 ) ) ;
#13701 = LOCAL_TIME ( 14, 11, 27.00000000000000000, #23410 ) ;
#13702 = CARTESIAN_POINT ( 'NONE',  ( -1.262685242559879909E-14, -17.30000000000000071, 2.500000000000000000 ) ) ;
#13703 = DIRECTION ( 'NONE',  ( 0.9730401042858024541, -0.2306359803922080898, -5.959266323863413074E-17 ) ) ;
#13704 = DIRECTION ( 'NONE',  ( 0.000000000000000000, 0.000000000000000000, -1.000000000000000000 ) ) ;
#13705 = CARTESIAN_POINT ( 'NONE',  ( 5.000000000000000000, -28.60000000000000142, 19.00000000000000000 ) ) ;
#13706 = DIRECTION ( 'NONE',  ( 1.304396158928310329E-15, 5.761557392270100456E-15, -1.000000000000000000 ) ) ;
#13707 = ORGANIZATION ( 'NAUO-ORG19', 'UNSPECIFIED', 'UNSPECIFIED' ) ;
#13708 =( REPRESENTATION_RELATIONSHIP ('NONE','NONE', #19303, #14436 ) REPRESENTATION_RELATIONSHIP_WITH_TRANSFORMATION ( #9126 )SHAPE_REPRESENTATION_RELATIONSHIP( ) );
#13709 = FACE_OUTER_BOUND ( 'NONE', #11655, .T. ) ;
#13710 = ORIENTED_EDGE ( 'NONE', *, *, #11082, .F. ) ;
#13711 = ORIENTED_EDGE ( 'NONE', *, *, #9076, .T. ) ;
#13712 = LINE ( 'NONE', #4696, #14145 ) ;
#13713 = DIRECTION ( 'NONE',  ( 2.270069654138865127E-15, 1.000000000000000000, -4.543838814073030634E-30 ) ) ;
#13714 = ORIENTED_EDGE ( 'NONE', *, *, #21146, .T. ) ;
#13715 = DIRECTION ( 'NONE',  ( 0.9730401042858036753, -0.2306359803922031493, 2.740969466505752002E-16 ) ) ;
#13716 = EDGE_CURVE ( 'NONE', #22023, #6032, #22872, .T. ) ;
#13717 = EDGE_LOOP ( 'NONE', ( #372, #21210, #9380, #2488 ) ) ;
#13718 = CC_DESIGN_APPROVAL ( #15029, ( #16771 ) ) ;
#13719 = CARTESIAN_POINT ( 'NONE',  ( 39.27359436029429673, 22.26288585089429972, 9.625000000000000000 ) ) ;
#13720 = PERSON_AND_ORGANIZATION ( #11966, #8758 ) ;
#13721 = AXIS2_PLACEMENT_3D ( 'NONE', #7228, #19464, #3194 ) ;
#13722 = DIRECTION ( 'NONE',  ( -1.000000000000000000, -6.662112528310618598E-09, 2.269018306577664942E-13 ) ) ;
#13723 = CIRCLE ( 'NONE', #15990, 0.3999999999999998557 ) ;
#13724 = CC_DESIGN_DATE_AND_TIME_ASSIGNMENT ( #12417, #1821, ( #22114 ) ) ;
#13725 = PRODUCT_DEFINITION ( 'UNKNOWN', '', #6135, #5173 ) ;
#13726 = CALENDAR_DATE ( 2026, 31, 10 ) ;
#13727 = SECURITY_CLASSIFICATION ( '', '', #11507 ) ;
#13728 = DIRECTION ( 'NONE',  ( 0.000000000000000000, 1.554450629062379680E-16, -1.000000000000000000 ) ) ;
#13729 = ADVANCED_FACE ( 'NONE', ( #19091 ), #20852, .F. ) ;
#13730 = EDGE_CURVE ( 'NONE', #10212, #14607, #12816, .T. ) ;
#13731 = LINE ( 'NONE', #20972, #18131 ) ;
#13732 = DIRECTION ( 'NONE',  ( -0.005235963827117092427, 0.9999862922474493931, 2.636227439667000721E-16 ) ) ;
#13733 = ORIENTED_EDGE ( 'NONE', *, *, #8699, .T. ) ;
#13734 = CARTESIAN_POINT ( 'NONE',  ( 43.84419854219520829, -33.09999999999999432, -21.50000000000000000 ) ) ;
#13735 = DESIGN_CONTEXT ( 'detailed design', #5972, 'design' ) ;
#13736 = LOCAL_TIME ( 14, 11, 27.00000000000000000, #12956 ) ;
#13737 = CARTESIAN_POINT ( 'NONE',  ( -20.18494928784681264, 20.45893982632658492, -5.499999999995553779 ) ) ;
#13738 = ORIENTED_EDGE ( 'NONE', *, *, #12571, .F. ) ;
#13739 = CARTESIAN_POINT ( 'NONE',  ( 35.12900133326353114, 11.79332846112002997, -8.806536740235884508 ) ) ;
#13740 = TOROIDAL_SURFACE ( 'NONE', #15243, 2.600000000000000089, 0.1000000000000000056 ) ;
#13741 = CARTESIAN_POINT ( 'NONE',  ( 34.40556712239430226, 8.514986143071229918, 27.68999999999999773 ) ) ;
#13742 = CALENDAR_DATE ( 2026, 31, 10 ) ;
#13743 = CIRCLE ( 'NONE', #11498, 12.49999999999999467 ) ;
#13744 = AXIS2_PLACEMENT_3D ( 'NONE', #7433, #21790, #12778 ) ;
#13745 = CARTESIAN_POINT ( 'NONE',  ( 118.4388045014059969, -7.086722380115130449, 18.89999999999999858 ) ) ;
#13746 = ORIENTED_EDGE ( 'NONE', *, *, #14700, .F. ) ;
#13747 = LOCAL_TIME ( 14, 11, 27.00000000000000000, #6379 ) ;
#13748 = ORIENTED_EDGE ( 'NONE', *, *, #19359, .T. ) ;
#13749 = COORDINATED_UNIVERSAL_TIME_OFFSET ( 0, 0, .AHEAD. ) ;
#13750 = CARTESIAN_POINT ( 'NONE',  ( -57.84992199990481510, 12.30077244250202462, 3.322570288448809374E-15 ) ) ;
#13751 = EDGE_CURVE ( 'NONE', #2375, #3635, #5279, .T. ) ;
#13752 = VERTEX_POINT ( 'NONE', #16099 ) ;
#13753 = AXIS2_PLACEMENT_3D ( 'NONE', #2739, #8676, #4867 ) ;
#13754 = FACE_OUTER_BOUND ( 'NONE', #531, .T. ) ;
#13755 = CALENDAR_DATE ( 2026, 31, 10 ) ;
#13756 = LOCAL_TIME ( 14, 11, 27.00000000000000000, #4021 ) ;
#13757 = CONTEXT_DEPENDENT_SHAPE_REPRESENTATION ( #13256, #2879 ) ;
#13758 = LINE ( 'NONE', #12112, #2481 ) ;
#13759 = AXIS2_PLACEMENT_3D ( 'NONE', #16269, #9150, #16387 ) ;
#13760 = EDGE_CURVE ( 'NONE', #15790, #14761, #10175, .T. ) ;
#13761 = AXIS2_PLACEMENT_3D ( 'NONE', #22250, #4100, #22504 ) ;
#13762 = EDGE_CURVE ( 'NONE', #8396, #7581, #7884, .T. ) ;
#13763 = AXIS2_PLACEMENT_3D ( 'NONE', #1728, #8992, #20374 ) ;
#13764 = CARTESIAN_POINT ( 'NONE',  ( 120.0770346556423931, 0.7635863056469410770, 13.00000000000000000 ) ) ;
#13765 = ORIENTED_EDGE ( 'NONE', *, *, #15937, .T. ) ;
#13766 = AXIS2_PLACEMENT_3D ( 'NONE', #11365, #3138, #2903 ) ;
#13767 = APPROVAL_ROLE ( '' ) ;
#13768 = VERTEX_POINT ( 'NONE', #8976 ) ;
#13769 = DIRECTION ( 'NONE',  ( 0.000000000000000000, 2.478176394252581338E-15, -1.000000000000000000 ) ) ;
#13770 = CARTESIAN_POINT ( 'NONE',  ( 102.8131131701580046, 7.202356331284469171, -13.00000000000000000 ) ) ;
#13771 = ORIENTED_EDGE ( 'NONE', *, *, #9827, .T. ) ;
#13772 = CIRCLE ( 'NONE', #9229, 3.499999999999999556 ) ;
#13773 = APPROVAL_PERSON_ORGANIZATION ( #4226, #14736, #7559 ) ;
#13774 = CARTESIAN_POINT ( 'NONE',  ( -19.49999999982379961, -0.1021026942259700004, -8.658030917271079259E-14 ) ) ;
#13775 = CARTESIAN_POINT ( 'NONE',  ( -62.73971250800079957, -25.32895006819559924, -5.000000000000000000 ) ) ;
#13776 = DIRECTION ( 'NONE',  ( 0.9730401042858035643, -0.2306359803922028717, -5.432877459303547053E-17 ) ) ;
#13777 = ORIENTED_EDGE ( 'NONE', *, *, #5598, .T. ) ;
#13778 = EDGE_LOOP ( 'NONE', ( #14466, #17449, #966, #6907 ) ) ;
#13779 = LINE ( 'NONE', #10225, #6846 ) ;
#13780 = VECTOR ( 'NONE', #10222, 1000.000000000000000 ) ;
#13781 = ORIENTED_EDGE ( 'NONE', *, *, #11286, .T. ) ;
#13782 = CIRCLE ( 'NONE', #18727, 6.499999999999997335 ) ;
#13783 = COORDINATED_UNIVERSAL_TIME_OFFSET ( 0, 0, .AHEAD. ) ;
#13784 = ADVANCED_FACE ( 'NONE', ( #19777 ), #10784, .T. ) ;
#13785 = ORIENTED_EDGE ( 'NONE', *, *, #15435, .T. ) ;
#13786 = CIRCLE ( 'NONE', #2024, 3.999999999999998668 ) ;
#13787 = ORIENTED_EDGE ( 'NONE', *, *, #23443, .T. ) ;
#13788 = CARTESIAN_POINT ( 'NONE',  ( 36.84099409957970295, 22.83947580187469839, -8.750000000000499156 ) ) ;
#13789 = PERSON_AND_ORGANIZATION ( #11966, #8758 ) ;
#13790 = CARTESIAN_POINT ( 'NONE',  ( -57.73978104676363898, -25.30277024906008521, 1.339745962155610037 ) ) ;
#13791 = AXIS2_PLACEMENT_3D ( 'NONE', #15560, #9798, #17020 ) ;
#13792 = EDGE_CURVE ( 'NONE', #12809, #16515, #18502, .T. ) ;
#13793 = CC_DESIGN_SECURITY_CLASSIFICATION ( #5821, ( #23478 ) ) ;
#13794 = AXIS2_PLACEMENT_3D ( 'NONE', #5433, #13040, #3754 ) ;
#13795 = EDGE_CURVE ( 'NONE', #8608, #11767, #20387, .T. ) ;
#13796 = CYLINDRICAL_SURFACE ( 'NONE', #870, 12.50000000000000533 ) ;
#13797 = AXIS2_PLACEMENT_3D ( 'NONE', #4213, #11932, #7781 ) ;
#13798 = CARTESIAN_POINT ( 'NONE',  ( -4.514225866272970400, 4.676725866273559795, -2.500000000000000000 ) ) ;
#13799 = PERSON_AND_ORGANIZATION_ROLE ( 'design_supplier' ) ;
#13800 = VECTOR ( 'NONE', #15050, 1000.000000000000000 ) ;
#13801 = ORIENTED_EDGE ( 'NONE', *, *, #4148, .T. ) ;
#13802 = DIRECTION ( 'NONE',  ( -0.5021071549687909918, 0.8648054144888007722, -3.074521526981951182E-17 ) ) ;
#13803 = LINE ( 'NONE', #15446, #10160 ) ;
#13804 = ORIENTED_EDGE ( 'NONE', *, *, #2576, .F. ) ;
#13805 = CARTESIAN_POINT ( 'NONE',  ( -17.00003426920497773, -0.08901278465814893570, -1.131420285898946938E-14 ) ) ;
#13806 = DIRECTION ( 'NONE',  ( 0.000000000000000000, -1.000000000000000000, 2.081668171172168119E-15 ) ) ;
#13807 = DIRECTION ( 'NONE',  ( 4.063875459488300452E-16, -1.011971878839179923E-16, -1.000000000000000000 ) ) ;
#13808 = EDGE_LOOP ( 'NONE', ( #3408, #5452, #13890, #6310, #18516, #8806, #7731, #9956, #5448, #9414, #2406, #7873 ) ) ;
#13809 = DIRECTION ( 'NONE',  ( 0.005235963827110212514, -0.9999862922474493931, 1.836993535195700665E-15 ) ) ;
#13810 = APPROVAL_ROLE ( '' ) ;
#13811 = VECTOR ( 'NONE', #18935, 1000.000000000000000 ) ;
#13812 = ORIENTED_EDGE ( 'NONE', *, *, #20388, .F. ) ;
#13813 = ORIENTED_EDGE ( 'NONE', *, *, #3850, .T. ) ;
#13814 = PLANE ( 'NONE',  #8104 ) ;
#13815 = CARTESIAN_POINT ( 'NONE',  ( -20.00000000000000000, -20.00000000000000000, -2.500000000000000000 ) ) ;
#13816 = ORIENTED_EDGE ( 'NONE', *, *, #11257, .T. ) ;
#13817 = VECTOR ( 'NONE', #2956, 1000.000000000000000 ) ;
#13818 = APPROVAL_STATUS ( 'not_yet_approved' ) ;
#13819 = CC_DESIGN_PERSON_AND_ORGANIZATION_ASSIGNMENT ( #11711, #2894, ( #10241 ) ) ;
#13820 = CARTESIAN_POINT ( 'NONE',  ( 113.4570673249340018, -28.10438863268850085, 2.700000000000049916 ) ) ;
#13821 = CARTESIAN_POINT ( 'NONE',  ( 31.37708959083939675, -0.2124270449898580104, -13.00000000000039968 ) ) ;
#13822 = CONTEXT_DEPENDENT_SHAPE_REPRESENTATION ( #3092, #22380 ) ;
#13823 = CYLINDRICAL_SURFACE ( 'NONE', #5981, 7.000000000000000000 ) ;
#13824 = SHAPE_REPRESENTATION_RELATIONSHIP ( 'NONE' , 'NONE' ,  #14436, #20135 ) ;
#13825 = DIRECTION ( 'NONE',  ( -0.2306359803922083396, -0.9730401042858023430, 0.000000000000000000 ) ) ;
#13826 = MECHANICAL_CONTEXT ( 'NONE', #17938, 'mechanical' ) ;
#13827 = CARTESIAN_POINT ( 'NONE',  ( 37.59139506199680625, 10.37158478572834142, 8.943038809424253444 ) ) ;
#13828 = DIRECTION ( 'NONE',  ( -2.270069654138870255E-15, -1.000000000000000000, -7.035747901516317327E-77 ) ) ;
#13829 = DIRECTION ( 'NONE',  ( -0.07397971354964408275, -0.9972597464969258363, 2.255140518769849223E-15 ) ) ;
#13830 = EDGE_CURVE ( 'NONE', #8186, #8149, #3700, .T. ) ;
#13831 = DIRECTION ( 'NONE',  ( -1.982541115402064913E-15, -6.938893903907227589E-15, 1.000000000000000000 ) ) ;
#13832 = FACE_OUTER_BOUND ( 'NONE', #14643, .T. ) ;
#13833 = ORIENTED_EDGE ( 'NONE', *, *, #1426, .T. ) ;
#13834 = DIRECTION ( 'NONE',  ( 0.005235963827117092427, -0.9999862922474493931, -2.636227439667000721E-16 ) ) ;
#13835 = ORIENTED_EDGE ( 'NONE', *, *, #14345, .F. ) ;
#13836 = PRODUCT_DEFINITION_SHAPE ( 'NONE', 'NONE',  #3293 ) ;
#13837 = ORIENTED_EDGE ( 'NONE', *, *, #19159, .T. ) ;
#13838 = CARTESIAN_POINT ( 'NONE',  ( -27.00000000000000000, -28.60000000000000142, 2.500000000000000000 ) ) ;
#13839 = DIRECTION ( 'NONE',  ( -0.005235963827110212514, 0.9999862922474493931, 5.936218956700083401E-19 ) ) ;
#13840 = ORIENTED_EDGE ( 'NONE', *, *, #530, .F. ) ;
#13841 = EDGE_CURVE ( 'NONE', #22271, #16628, #6757, .T. ) ;
#13842 = FACE_OUTER_BOUND ( 'NONE', #13157, .T. ) ;
#13843 = VERTEX_POINT ( 'NONE', #23442 ) ;
#13844 = DIRECTION ( 'NONE',  ( -9.594916218540590128E-33, 2.583840697242805182E-16, -1.000000000000000000 ) ) ;
#13845 = APPROVAL_ROLE ( '' ) ;
#13846 = DIRECTION ( 'NONE',  ( -0.9730401042858024541, 0.2306359803922080898, 5.959266323858942451E-17 ) ) ;
#13847 =( REPRESENTATION_RELATIONSHIP ('NONE','NONE', #19303, #9605 ) REPRESENTATION_RELATIONSHIP_WITH_TRANSFORMATION ( #10298 )SHAPE_REPRESENTATION_RELATIONSHIP( ) );
#13848 = AXIS2_PLACEMENT_3D ( 'NONE', #15404, #21103, #15525 ) ;
#13849 = ITEM_DEFINED_TRANSFORMATION ( 'NONE', 'NONE', #15170,  #12739 ) ;
#13850 = DIRECTION ( 'NONE',  ( 1.000000000000000000, 0.000000000000000000, 0.000000000000000000 ) ) ;
#13851 = PLANE ( 'NONE',  #8471 ) ;
#13852 = DIRECTION ( 'NONE',  ( 0.000000000000000000, 0.000000000000000000, -1.000000000000000000 ) ) ;
#13853 = LINE ( 'NONE', #22738, #6233 ) ;
#13854 = ORIENTED_EDGE ( 'NONE', *, *, #1595, .F. ) ;
#13855 = PLANE ( 'NONE',  #23408 ) ;
#13856 = EDGE_CURVE ( 'NONE', #12721, #21501, #9023, .T. ) ;
#13857 = CIRCLE ( 'NONE', #3235, 2.499999999999999112 ) ;
#13858 = ORIENTED_EDGE ( 'NONE', *, *, #6331, .F. ) ;
#13859 = DIRECTION ( 'NONE',  ( 0.000000000000000000, 0.000000000000000000, 1.000000000000000000 ) ) ;
#13860 = CC_DESIGN_DATE_AND_TIME_ASSIGNMENT ( #9592, #8034, ( #13355 ) ) ;
#13861 = COORDINATED_UNIVERSAL_TIME_OFFSET ( 0, 0, .AHEAD. ) ;
#13862 = CARTESIAN_POINT ( 'NONE',  ( 114.6158348783805963, -5.872266427260702137, 3.471470530880454566E-14 ) ) ;
#13863 = ORIENTED_EDGE ( 'NONE', *, *, #5288, .T. ) ;
#13864 = VERTEX_POINT ( 'NONE', #19900 ) ;
#13865 = ADVANCED_FACE ( 'NONE', ( #7196 ), #8652, .F. ) ;
#13866 = EDGE_CURVE ( 'NONE', #8755, #4894, #12668, .T. ) ;
#13867 = PERSON_AND_ORGANIZATION ( #11966, #8758 ) ;
#13868 = DIRECTION ( 'NONE',  ( 0.9999862922474493931, 0.005235963827110211646, 1.541976423090501796E-16 ) ) ;
#13869 = EDGE_LOOP ( 'NONE', ( #17190, #23014, #12264, #507, #4251 ) ) ;
#13870 = LINE ( 'NONE', #12109, #10186 ) ;
#13871 = PERSON_AND_ORGANIZATION ( #11966, #8758 ) ;
#13872 = DATE_TIME_ROLE ( 'classification_date' ) ;
#13873 = DIRECTION ( 'NONE',  ( -0.9730401042858036753, 0.2306359803922028995, 5.958148513035547083E-17 ) ) ;
#13874 = CONICAL_SURFACE ( 'NONE', #975, 2.283500000000000085, 0.7853981633974447263 ) ;
#13875 = CARTESIAN_POINT ( 'NONE',  ( -19.49999999982360066, -0.1021026942259700004, -2.500000000000000000 ) ) ;
#13876 = EDGE_LOOP ( 'NONE', ( #5477, #15310 ) ) ;
#13877 = EDGE_CURVE ( 'NONE', #10197, #6181, #19260, .T. ) ;
#13878 = ORIENTED_EDGE ( 'NONE', *, *, #1144, .T. ) ;
#13879 = LINE ( 'NONE', #19227, #1178 ) ;
#13880 = CARTESIAN_POINT ( 'NONE',  ( 43.45766680872420551, 21.27115113520920175, 13.00000000000000000 ) ) ;
#13881 = ORIENTED_EDGE ( 'NONE', *, *, #10531, .F. ) ;
#13882 = CC_DESIGN_PERSON_AND_ORGANIZATION_ASSIGNMENT ( #9259, #12925, ( #18095 ) ) ;
#13883 = DIRECTION ( 'NONE',  ( -1.187319687680494078E-16, -2.805478249478340539E-20, -1.000000000000000000 ) ) ;
#13884 = PRODUCT_DEFINITION ( 'UNKNOWN', '', #6875, #4942 ) ;
#13885 = CARTESIAN_POINT ( 'NONE',  ( 34.94102482032229773, 25.66320561742200113, -13.00000000000049916 ) ) ;
#13886 = CARTESIAN_POINT ( 'NONE',  ( -19.99975861755300244, 22.95209442650120124, 3.749999999999900080 ) ) ;
#13887 = EDGE_LOOP ( 'NONE', ( #9866, #21882 ) ) ;
#13888 = VERTEX_POINT ( 'NONE', #21898 ) ;
#13889 = CARTESIAN_POINT ( 'NONE',  ( -62.93867965702761325, 12.67062903583649991, 3.427095671567209849E-15 ) ) ;
#13890 = ORIENTED_EDGE ( 'NONE', *, *, #7006, .F. ) ;
#13891 = EDGE_CURVE ( 'NONE', #15201, #9834, #16573, .T. ) ;
#13892 = EDGE_CURVE ( 'NONE', #15778, #15790, #1830, .T. ) ;
#13893 = APPROVAL_DATE_TIME ( #1170, #6196 ) ;
#13894 = AXIS2_PLACEMENT_3D ( 'NONE', #16026, #10477, #10590 ) ;
#13895 = ORIENTED_EDGE ( 'NONE', *, *, #21731, .T. ) ;
#13896 = ORIENTED_EDGE ( 'NONE', *, *, #16160, .F. ) ;
#13897 = FACE_OUTER_BOUND ( 'NONE', #14846, .T. ) ;
#13898 = DATE_AND_TIME ( #17814, #18681 ) ;
#13899 = CARTESIAN_POINT ( 'NONE',  ( -15.00000000000000000, -20.00000000000000000, 2.500000000000000000 ) ) ;
#13900 = AXIS2_PLACEMENT_3D ( 'NONE', #9120, #14692, #16353 ) ;
#13901 = AXIS2_PLACEMENT_3D ( 'NONE', #20474, #4342, #18833 ) ;
#13902 = CARTESIAN_POINT ( 'NONE',  ( 34.85715660638719982, 8.407947612062049103, -27.55602540378494325 ) ) ;
#13903 = DIRECTION ( 'NONE',  ( 1.138590270679734009E-14, 2.220446049251240387E-15, 1.000000000000000000 ) ) ;
#13904 = APPROVAL_STATUS ( 'not_yet_approved' ) ;
#13905 = EDGE_CURVE ( 'NONE', #18815, #14761, #7087, .T. ) ;
#13906 = VERTEX_POINT ( 'NONE', #14556 ) ;
#13907 = DIRECTION ( 'NONE',  ( -0.9730401042858035643, 0.2306359803922028717, 5.667427308550587516E-17 ) ) ;
#13908 = LINE ( 'NONE', #22681, #16203 ) ;
#13909 = ORIENTED_EDGE ( 'NONE', *, *, #7121, .F. ) ;
#13910 = ADVANCED_BREP_SHAPE_REPRESENTATION ( '', ( #1851, #12739 ), #7801 ) ;
#13911 = EDGE_CURVE ( 'NONE', #928, #18213, #13959, .T. ) ;
#13912 = CARTESIAN_POINT ( 'NONE',  ( -17.47493719149860070, 26.45208920939580111, -7.999999999996139088 ) ) ;
#13913 = DIRECTION ( 'NONE',  ( 0.005235964011411631258, -0.9999862922464843873, 2.602085213965210642E-15 ) ) ;
#13914 = FACE_OUTER_BOUND ( 'NONE', #10335, .T. ) ;
#13915 = ORIENTED_EDGE ( 'NONE', *, *, #15468, .F. ) ;
#13916 = DIRECTION ( 'NONE',  ( 0.9730401042858036753, -0.2306359803922031493, -5.432877459303553216E-17 ) ) ;
#13917 = EDGE_CURVE ( 'NONE', #4216, #16805, #16547, .T. ) ;
#13918 = PERSON_AND_ORGANIZATION ( #11966, #8758 ) ;
#13919 = VECTOR ( 'NONE', #11983, 1000.000000000000000 ) ;
#13921 = EDGE_CURVE ( 'NONE', #6893, #10522, #16376, .T. ) ;
#13920 = ORIENTED_EDGE ( 'NONE', *, *, #18496, .T. ) ;
#13922 = ORIENTED_EDGE ( 'NONE', *, *, #5492, .T. ) ;
#13923 = CARTESIAN_POINT ( 'NONE',  ( 114.3964932440919995, -22.26358663789240211, 13.00000000000000000 ) ) ;
#13924 = CARTESIAN_POINT ( 'NONE',  ( 29.36184298829660122, -3.294841866349869974, -15.00000000000039968 ) ) ;
#13925 = VECTOR ( 'NONE', #9666, 999.9999999999998863 ) ;
#13926 = PLANE ( 'NONE',  #20168 ) ;
#13927 = DATE_TIME_ROLE ( 'classification_date' ) ;
#13928 = CARTESIAN_POINT ( 'NONE',  ( -25.44879460632040136, 25.46418757447539960, -3.750000000000069722 ) ) ;
#13929 = DIRECTION ( 'NONE',  ( -0.005235963827108362431, 0.9999862922474493931, 5.936218956694023463E-19 ) ) ;
#13930 = CARTESIAN_POINT ( 'NONE',  ( 34.89491389100810181, 23.30074776265910330, -8.750000000000499156 ) ) ;
#13931 = CIRCLE ( 'NONE', #10154, 2.009240000000000581 ) ;
#13932 = ORIENTED_EDGE ( 'NONE', *, *, #8112, .F. ) ;
#13933 = DIRECTION ( 'NONE',  ( 2.269747459788990007E-13, 2.220446049250330436E-15, 1.000000000000000000 ) ) ;
#13934 = CALENDAR_DATE ( 2026, 31, 10 ) ;
#13935 = CIRCLE ( 'NONE', #5218, 2.500000000000000444 ) ;
#13936 = AXIS2_PLACEMENT_3D ( 'NONE', #4653, #8456, #8110 ) ;
#13937 = DIRECTION ( 'NONE',  ( -8.623081276789554834E-17, -1.054188326053478339E-16, -1.000000000000000000 ) ) ;
#13938 = LINE ( 'NONE', #22836, #9770 ) ;
#13939 = CC_DESIGN_PERSON_AND_ORGANIZATION_ASSIGNMENT ( #3327, #17600, ( #7231 ) ) ;
#13940 = CARTESIAN_POINT ( 'NONE',  ( 117.1011158151309957, -12.73035498497280038, 20.00000000000000000 ) ) ;
#13941 = DIRECTION ( 'NONE',  ( 2.270069654138865127E-15, 1.000000000000000000, -4.543838814073030634E-30 ) ) ;
#13942 = CARTESIAN_POINT ( 'NONE',  ( -26.68810977484059777, -6.639828994528159889, -8.572666733291279949E-14 ) ) ;
#13943 = ORIENTED_EDGE ( 'NONE', *, *, #11001, .T. ) ;
#13944 = DIRECTION ( 'NONE',  ( -1.751019220569994795E-16, -2.300154215587015208E-15, -1.000000000000000000 ) ) ;
#13945 = ORIENTED_EDGE ( 'NONE', *, *, #17978, .T. ) ;
#13946 = ORIENTED_EDGE ( 'NONE', *, *, #4988, .T. ) ;
#13947 = DIRECTION ( 'NONE',  ( -0.9730401042858022320, 0.2306359803922080343, 5.959266323858941219E-17 ) ) ;
#13948 = DIRECTION ( 'NONE',  ( -0.000000000000000000, 1.000000000000000000, 0.000000000000000000 ) ) ;
#13949 = ORIENTED_EDGE ( 'NONE', *, *, #10290, .T. ) ;
#13950 = CARTESIAN_POINT ( 'NONE',  ( -31.64160538070510142, 6.334412527122569969, -3.750000000000000000 ) ) ;
#13951 = VECTOR ( 'NONE', #11740, 1000.000000000000000 ) ;
#13952 = ORIENTED_EDGE ( 'NONE', *, *, #20170, .F. ) ;
#13953 = FACE_BOUND ( 'NONE', #6359, .T. ) ;
#13954 = CIRCLE ( 'NONE', #3703, 2.499999999999998668 ) ;
#13955 = PERSON_AND_ORGANIZATION ( #11966, #8758 ) ;
#13956 = FACE_OUTER_BOUND ( 'NONE', #21756, .T. ) ;
#13957 = EDGE_CURVE ( 'NONE', #14674, #15708, #19647, .T. ) ;
#13958 = APPROVAL_STATUS ( 'not_yet_approved' ) ;
#13959 =( BOUNDED_CURVE ( )  B_SPLINE_CURVE ( 2, ( #12773, #20010, #20124 ),
 .UNSPECIFIED., .F., .F. ) 
 B_SPLINE_CURVE_WITH_KNOTS ( ( 3, 3 ),
 ( 0.000000000000000000, 0.1168436138077847686 ),
 .UNSPECIFIED. ) 
 CURVE ( )  GEOMETRIC_REPRESENTATION_ITEM ( )  RATIONAL_B_SPLINE_CURVE ( ( 1.000000000000000000, 1.077350269189619514, 1.077350269189624843 ) ) 
 REPRESENTATION_ITEM ( '' )  );
#13960 = AXIS2_PLACEMENT_3D ( 'NONE', #21343, #10672, #3749 ) ;
#13961 = DIRECTION ( 'NONE',  ( -0.9999862922464843873, -0.005235964011397749134, 0.000000000000000000 ) ) ;
#13962 = DIRECTION ( 'NONE',  ( -1.000000000000000000, -9.259491321837100239E-11, 2.269596547736281384E-13 ) ) ;
#13963 = CARTESIAN_POINT ( 'NONE',  ( 0.000000000000000000, 0.000000000000000000, 0.000000000000000000 ) ) ;
#13964 = CIRCLE ( 'NONE', #23427, 0.3999999999999982458 ) ;
#13965 = DIRECTION ( 'NONE',  ( 6.124378941433959925E-17, 0.000000000000000000, 1.000000000000000000 ) ) ;
#13966 = ORIENTED_EDGE ( 'NONE', *, *, #19947, .T. ) ;
#13967 = CARTESIAN_POINT ( 'NONE',  ( -62.73971250800079957, -25.32895006819559924, -5.538452170245418869E-15 ) ) ;
#13968 = DESIGN_CONTEXT ( 'detailed design', #21439, 'design' ) ;
#13969 = CARTESIAN_POINT ( 'NONE',  ( -19.49999999982379961, -0.1021026942259709996, 9.160072195675308484E-14 ) ) ;
#13970 = AXIS2_PLACEMENT_3D ( 'NONE', #8243, #21059, #4789 ) ;
#13971 = EDGE_LOOP ( 'NONE', ( #16894, #16609, #2465, #7030 ) ) ;
#13972 = DIRECTION ( 'NONE',  ( -7.008869410147150310E-16, 5.150359455772420684E-15, 1.000000000000000000 ) ) ;
#13973 = CARTESIAN_POINT ( 'NONE',  ( -20.00000000000000000, -20.00000000000000000, 2.500000000000000000 ) ) ;
#13974 = ORIENTED_EDGE ( 'NONE', *, *, #22742, .T. ) ;
#13975 = COORDINATED_UNIVERSAL_TIME_OFFSET ( 0, 0, .AHEAD. ) ;
#13976 = PLANE ( 'NONE',  #6984 ) ;
#13977 = VERTEX_POINT ( 'NONE', #20472 ) ;
#13978 = ORIENTED_EDGE ( 'NONE', *, *, #555, .T. ) ;
#13979 = APPLICATION_CONTEXT ( 'configuration controlled 3d designs of mechanical parts and assemblies' ) ;
#13980 = APPLICATION_PROTOCOL_DEFINITION ( 'international standard', 'config_control_design', 1994, #4758 ) ;
#13981 = CARTESIAN_POINT ( 'NONE',  ( 117.0319250210129951, -13.02226701625849969, -18.89999999999999858 ) ) ;
#13982 = ORIENTED_EDGE ( 'NONE', *, *, #9141, .T. ) ;
#13983 = FACE_OUTER_BOUND ( 'NONE', #14729, .T. ) ;
#13984 = CALENDAR_DATE ( 2026, 31, 10 ) ;
#13985 = EDGE_CURVE ( 'NONE', #4748, #8216, #13477, .T. ) ;
#13986 = AXIS2_PLACEMENT_3D ( 'NONE', #13798, #4409, #16994 ) ;
#13987 = CARTESIAN_POINT ( 'NONE',  ( -20.00000000397430000, 22.95208919257349933, -6.749999999995570654 ) ) ;
#13988 = FACE_OUTER_BOUND ( 'NONE', #7983, .T. ) ;
#13989 = ORIENTED_EDGE ( 'NONE', *, *, #18644, .T. ) ;
#13990 = EDGE_CURVE ( 'NONE', #12386, #17514, #22328, .T. ) ;
#13991 = EDGE_CURVE ( 'NONE', #2851, #21488, #2193, .T. ) ;
#13992 = ORIENTED_EDGE ( 'NONE', *, *, #1252, .T. ) ;
#13993 = CARTESIAN_POINT ( 'NONE',  ( -14.00000000144900092, -4.350228928435750042, -6.749999999996870059 ) ) ;
#13994 = FACE_OUTER_BOUND ( 'NONE', #11930, .T. ) ;
#13995 = VERTEX_POINT ( 'NONE', #4341 ) ;
#13996 = CARTESIAN_POINT ( 'NONE',  ( -19.49999999982360066, -0.1021026942259700004, -1.101737663870589950E-14 ) ) ;
#13997 = ADVANCED_FACE ( 'NONE', ( #18936 ), #11484, .T. ) ;
#13998 = DIRECTION ( 'NONE',  ( 0.9730401042858035643, -0.2306359803922028717, -5.959266323858674978E-17 ) ) ;
#13999 = ORIENTED_EDGE ( 'NONE', *, *, #1779, .F. ) ;
#14000 = ORIENTED_EDGE ( 'NONE', *, *, #22125, .T. ) ;
#14001 = CARTESIAN_POINT ( 'NONE',  ( 33.27705887009660302, -3.036156860536499913, 13.00000000000000000 ) ) ;
#14002 = EDGE_LOOP ( 'NONE', ( #9467, #18375, #8159, #4915 ) ) ;
#14003 = APPROVAL_DATE_TIME ( #8197, #10713 ) ;
#14004 = ORIENTED_EDGE ( 'NONE', *, *, #2122, .F. ) ;
#14005 = ORIENTED_EDGE ( 'NONE', *, *, #8804, .T. ) ;
#14006 = DIRECTION ( 'NONE',  ( 1.040345436475888435E-32, 1.169424102322700040E-16, 1.000000000000000000 ) ) ;
#14007 = ORGANIZATION ( 'NAUO-ORG7', 'UNSPECIFIED', 'UNSPECIFIED' ) ;
#14008 = APPLICATION_PROTOCOL_DEFINITION ( 'international standard', 'config_control_design', 1994, #5520 ) ;
#14009 = EDGE_CURVE ( 'NONE', #21124, #20573, #9919, .T. ) ;
#14010 = CARTESIAN_POINT ( 'NONE',  ( -31.64153798721130428, 6.334539654120280083, 3.750000000000000000 ) ) ;
#14011 = CC_DESIGN_PERSON_AND_ORGANIZATION_ASSIGNMENT ( #14572, #19919, ( #14534 ) ) ;
#14012 = APPROVAL ( #8290, 'UNSPECIFIED' ) ;
#14013 = CARTESIAN_POINT ( 'NONE',  ( -31.64153798721130428, 6.334539654120280083, 2.500000000000000000 ) ) ;
#14014 = EDGE_CURVE ( 'NONE', #19785, #10728, #14338, .T. ) ;
#14015 = EDGE_CURVE ( 'NONE', #9841, #9664, #18719, .T. ) ;
#14016 = APPLICATION_PROTOCOL_DEFINITION ( 'international standard', 'config_control_design', 1994, #2602 ) ;
#14017 = PRODUCT_DEFINITION_SHAPE ( 'NONE', 'NONE',  #22291 ) ;
#14018 = CC_DESIGN_PERSON_AND_ORGANIZATION_ASSIGNMENT ( #8071, #9857, ( #20866 ) ) ;
#14019 = ORIENTED_EDGE ( 'NONE', *, *, #18059, .T. ) ;
#14020 =( GEOMETRIC_REPRESENTATION_CONTEXT ( 3 ) GLOBAL_UNCERTAINTY_ASSIGNED_CONTEXT ( ( #6826 ) ) GLOBAL_UNIT_ASSIGNED_CONTEXT ( ( #13320, #10237, #16992 ) ) REPRESENTATION_CONTEXT ( 'NONE', 'WORKASPACE' ) );
#14021 = DIRECTION ( 'NONE',  ( 0.9949874374308178560, 0.09999999677427207079, -1.144917494144692682E-14 ) ) ;
#14022 = EDGE_CURVE ( 'NONE', #9363, #17821, #2439, .T. ) ;
#14023 = AXIS2_PLACEMENT_3D ( 'NONE', #18787, #9392, #6179 ) ;
#14024 = DIRECTION ( 'NONE',  ( -0.9730401042858035643, 0.2306359803922028717, -2.804983810440357322E-16 ) ) ;
#14025 = ORIENTED_EDGE ( 'NONE', *, *, #4604, .T. ) ;
#14026 = DIRECTION ( 'NONE',  ( -6.662161100567945949E-09, 1.000000000000000000, -2.220444537107962377E-15 ) ) ;
#14027 = CYLINDRICAL_SURFACE ( 'NONE', #14555, 1.000000000000000000 ) ;
#14028 = DIRECTION ( 'NONE',  ( -2.270069654138865127E-15, -1.000000000000000000, -4.543838814073030634E-30 ) ) ;
#14029 = ORIENTED_EDGE ( 'NONE', *, *, #18904, .F. ) ;
#14030 = AXIS2_PLACEMENT_3D ( 'NONE', #18593, #2309, #17278 ) ;
#14031 = DIRECTION ( 'NONE',  ( 2.269747459789000104E-13, 2.220446049250330436E-15, 1.000000000000000000 ) ) ;
#14032 = APPROVAL_ROLE ( '' ) ;
#14033 = ORIENTED_EDGE ( 'NONE', *, *, #10182, .F. ) ;
#14034 = ORIENTED_EDGE ( 'NONE', *, *, #619, .F. ) ;
#14035 = CARTESIAN_POINT ( 'NONE',  ( 1.045027777644792710, 20.68729090833368289, -7.053516793552093206E-15 ) ) ;
#14036 = DIRECTION ( 'NONE',  ( 0.000000000000000000, 0.000000000000000000, 1.000000000000000000 ) ) ;
#14037 = CARTESIAN_POINT ( 'NONE',  ( -0.5391976746803449627, 18.33937061236850141, -7.621247264287879719E-15 ) ) ;
#14038 = APPROVAL_DATE_TIME ( #6806, #22560 ) ;
#14039 = EDGE_CURVE ( 'NONE', #11256, #14790, #3812, .T. ) ;
#14040 = CC_DESIGN_APPROVAL ( #574, ( #7977 ) ) ;
#14041 = CARTESIAN_POINT ( 'NONE',  ( 27.03882233449090222, -4.640652085158520457, -20.00000000000000000 ) ) ;
#14042 = CIRCLE ( 'NONE', #3782, 2.500000000000000444 ) ;
#14043 = CARTESIAN_POINT ( 'NONE',  ( -62.93867965702758482, 12.67062903583650169, -2.999765877365338174 ) ) ;
#14044 = DIRECTION ( 'NONE',  ( 0.000000000000000000, 0.000000000000000000, 1.000000000000000000 ) ) ;
#14045 = VECTOR ( 'NONE', #16755, 1000.000000000000000 ) ;
#14046 = ADVANCED_FACE ( 'NONE', ( #15122 ), #7543, .T. ) ;
#14047 = ADVANCED_FACE ( 'NONE', ( #11243 ), #1050, .F. ) ;
#14048 = EDGE_LOOP ( 'NONE', ( #3251, #12550, #8315, #16001 ) ) ;
#14049 = FACE_OUTER_BOUND ( 'NONE', #6149, .T. ) ;
#14050 = DATE_AND_TIME ( #5370, #14091 ) ;
#14051 = CARTESIAN_POINT ( 'NONE',  ( 36.56346929822891667, 7.944129105593864537, 8.864692334380281480 ) ) ;
#14052 = CYLINDRICAL_SURFACE ( 'NONE', #22631, 6.500000000000000000 ) ;
#14053 = LINE ( 'NONE', #21174, #4028 ) ;
#14054 = SECURITY_CLASSIFICATION ( '', '', #6686 ) ;
#14055 = DIRECTION ( 'NONE',  ( -0.2306359803922028995, -0.9730401042858035643, -1.064172857958375654E-32 ) ) ;
#14056 = DIRECTION ( 'NONE',  ( 0.005235963827108352890, -0.9999862922474493931, -2.671135040551771006E-18 ) ) ;
#14057 = EDGE_LOOP ( 'NONE', ( #10206, #19731, #4268, #4043, #20630, #4588, #23016, #23226 ) ) ;
#14058 = CARTESIAN_POINT ( 'NONE',  ( -32.42721070416779838, 10.33414378941739997, -2.500000000000000000 ) ) ;
#14059 = ORIENTED_EDGE ( 'NONE', *, *, #10155, .T. ) ;
#14060 = CYLINDRICAL_SURFACE ( 'NONE', #20609, 4.750000000000000000 ) ;
#14061 = CARTESIAN_POINT ( 'NONE',  ( -62.82872441665805496, -8.329083101359751495, -5.528360538656856695E-15 ) ) ;
#14062 = ORIENTED_EDGE ( 'NONE', *, *, #11631, .F. ) ;
#14063 = AXIS2_PLACEMENT_3D ( 'NONE', #3097, #17251, #19150 ) ;
#14064 = CARTESIAN_POINT ( 'NONE',  ( 120.8143550994449953, 2.935590694028629599, 20.00000000000000000 ) ) ;
#14066 = EDGE_LOOP ( 'NONE', ( #16502, #18863 ) ) ;
#14065 = EDGE_CURVE ( 'NONE', #18882, #17890, #20780, .T. ) ;
#14067 = CARTESIAN_POINT ( 'NONE',  ( -62.86014019962070165, -2.329165347875060021, -5.524798807282839984E-15 ) ) ;
#14068 = APPROVAL_DATE_TIME ( #2912, #21986 ) ;
#14069 = CYLINDRICAL_SURFACE ( 'NONE', #17741, 2.066999999999997062 ) ;
#14070 = SECURITY_CLASSIFICATION ( '', '', #13654 ) ;
#14071 = EDGE_CURVE ( 'NONE', #13532, #2445, #7654, .T. ) ;
#14072 =( NAMED_UNIT ( * ) SI_UNIT ( $, .STERADIAN. ) SOLID_ANGLE_UNIT ( ) );
#14073 = APPROVAL_PERSON_ORGANIZATION ( #1174, #19836, #3431 ) ;
#14074 = CARTESIAN_POINT ( 'NONE',  ( 36.68971944905815974, 14.39675017681084945, -26.50000000000052225 ) ) ;
#14075 = EDGE_CURVE ( 'NONE', #7803, #16383, #11606, .T. ) ;
#14076 = AXIS2_PLACEMENT_3D ( 'NONE', #4479, #20858, #4595 ) ;
#14077 = FACE_OUTER_BOUND ( 'NONE', #11451, .T. ) ;
#14078 = CARTESIAN_POINT ( 'NONE',  ( 0.000000000000000000, 0.000000000000000000, 0.000000000000000000 ) ) ;
#14079 = CARTESIAN_POINT ( 'NONE',  ( 37.10730959030829723, 23.96304573415810069, -11.00000000000049916 ) ) ;
#14080 = DIRECTION ( 'NONE',  ( 0.1630842657209355673, 0.6880432561069612651, 0.7071067811865432429 ) ) ;
#14081 = ORIENTED_EDGE ( 'NONE', *, *, #12356, .T. ) ;
#14082 = CARTESIAN_POINT ( 'NONE',  ( -22.50000000000180123, -20.00000001665528160, -7.999999999994901856 ) ) ;
#14083 = DIRECTION ( 'NONE',  ( 0.000000000000000000, 2.478176394252581338E-15, -1.000000000000000000 ) ) ;
#14084 = ORIENTED_EDGE ( 'NONE', *, *, #3850, .F. ) ;
#14085 = CARTESIAN_POINT ( 'NONE',  ( -26.75617730459320143, 6.359992804688680224, -8.571895024826909188E-14 ) ) ;
#14086 = CARTESIAN_POINT ( 'NONE',  ( -14.00000000202540029, 1.899127378930369980, 5.500000000004440004 ) ) ;
#14087 = ORIENTED_EDGE ( 'NONE', *, *, #9826, .F. ) ;
#14088 = PRODUCT_DEFINITION_FORMATION_WITH_SPECIFIED_SOURCE ( 'ANY', '', #21034, .NOT_KNOWN. ) ;
#14089 = DATE_AND_TIME ( #23336, #19773 ) ;
#14090 = LINE ( 'NONE', #3175, #20628 ) ;
#14091 = LOCAL_TIME ( 14, 11, 27.00000000000000000, #5142 ) ;
#14092 = ORIENTED_EDGE ( 'NONE', *, *, #9185, .T. ) ;
#14093 = ORIENTED_EDGE ( 'NONE', *, *, #8181, .F. ) ;
#14094 = CIRCLE ( 'NONE', #12222, 6.499999999999997335 ) ;
#14095 = APPLICATION_PROTOCOL_DEFINITION ( 'international standard', 'config_control_design', 1994, #5333 ) ;
#14096 = CARTESIAN_POINT ( 'NONE',  ( -16.50058068176721804, 23.02794805996685668, 2.499999999999900524 ) ) ;
#14097 = VERTEX_POINT ( 'NONE', #6104 ) ;
#14098 = DIRECTION ( 'NONE',  ( 0.9730401042858024541, -0.2306359803922080898, -5.959266323858472832E-17 ) ) ;
#14099 = LOCAL_TIME ( 14, 11, 27.00000000000000000, #2568 ) ;
#14100 = APPLICATION_PROTOCOL_DEFINITION ( 'international standard', 'config_control_design', 1994, #20803 ) ;
#14101 = CC_DESIGN_PERSON_AND_ORGANIZATION_ASSIGNMENT ( #16408, #10506, ( #8771 ) ) ;
#14102 = COORDINATED_UNIVERSAL_TIME_OFFSET ( 0, 0, .AHEAD. ) ;
#14103 = CARTESIAN_POINT ( 'NONE',  ( -3.499952022866071211, -0.01832587339492825623, 8.925353670776949322E-14 ) ) ;
#14104 = APPROVAL_PERSON_ORGANIZATION ( #13542, #13443, #4165 ) ;
#14105 = DIRECTION ( 'NONE',  ( -0.9999862922474491711, -0.005235963827128302210, 1.239088197126291310E-16 ) ) ;
#14106 = VECTOR ( 'NONE', #21177, 1000.000000000000000 ) ;
#14107 = EDGE_LOOP ( 'NONE', ( #23020, #22506, #10306, #597 ) ) ;
#14108 = VECTOR ( 'NONE', #8408, 1000.000000000000000 ) ;
#14109 = CIRCLE ( 'NONE', #3867, 2.999999999999999556 ) ;
#14110 = ORIENTED_EDGE ( 'NONE', *, *, #10434, .F. ) ;
#14111 = LOCAL_TIME ( 14, 11, 27.00000000000000000, #22168 ) ;
#14112 = CARTESIAN_POINT ( 'NONE',  ( 39.69419854219519550, 9.774809681453278998, 25.00000000000000000 ) ) ;
#14113 = FACE_OUTER_BOUND ( 'NONE', #22228, .T. ) ;
#14114 = EDGE_LOOP ( 'NONE', ( #10545, #19802, #12079, #8720, #18919, #9040 ) ) ;
#14115 = AXIS2_PLACEMENT_3D ( 'NONE', #18094, #20096, #7065 ) ;
#14116 = EDGE_CURVE ( 'NONE', #8586, #12727, #13357, .T. ) ;
#14117 = AXIS2_PLACEMENT_3D ( 'NONE', #14847, #4292, #4044 ) ;
#14118 = DIRECTION ( 'NONE',  ( -1.173102895937339952E-16, -2.365413804416879953E-16, -1.000000000000000000 ) ) ;
#14119 = CARTESIAN_POINT ( 'NONE',  ( 36.90701083165220098, 10.61980902621680123, -29.25000000000050093 ) ) ;
#14120 = VERTEX_POINT ( 'NONE', #22492 ) ;
#14121 = ORIENTED_EDGE ( 'NONE', *, *, #11145, .F. ) ;
#14122 = ORIENTED_EDGE ( 'NONE', *, *, #2387, .F. ) ;
#14123 = DATE_TIME_ROLE ( 'classification_date' ) ;
#14124 = PRODUCT_DEFINITION_FORMATION_WITH_SPECIFIED_SOURCE ( 'ANY', '', #14605, .NOT_KNOWN. ) ;
#14125 = ORIENTED_EDGE ( 'NONE', *, *, #14245, .F. ) ;
#14126 = ORIENTED_EDGE ( 'NONE', *, *, #20787, .T. ) ;
#14127 = CARTESIAN_POINT ( 'NONE',  ( 1.305890168459409084, 26.12369144665493437, -4.914342747878582431E-18 ) ) ;
#14128 = COORDINATED_UNIVERSAL_TIME_OFFSET ( 0, 0, .AHEAD. ) ;
#14129 = VECTOR ( 'NONE', #21734, 1000.000000000000227 ) ;
#14130 = ADVANCED_FACE ( 'NONE', ( #4091 ), #17757, .F. ) ;
#14131 = CIRCLE ( 'NONE', #23221, 2.750000000000002220 ) ;
#14132 = EDGE_CURVE ( 'NONE', #18750, #12797, #8599, .T. ) ;
#14133 = CARTESIAN_POINT ( 'NONE',  ( 33.27705887009660302, -3.036156860536515012, 13.00000000000000000 ) ) ;
#14134 = AXIS2_PLACEMENT_3D ( 'NONE', #11487, #11610, #20608 ) ;
#14136 = AXIS2_PLACEMENT_3D ( 'NONE', #22175, #9484, #18770 ) ;
#14135 = DIRECTION ( 'NONE',  ( -2.269700743865584947E-13, -2.220446049247695246E-15, -1.000000000000000000 ) ) ;
#14137 = AXIS2_PLACEMENT_3D ( 'NONE', #11192, #9266, #13069 ) ;
#14138 = DATE_AND_TIME ( #8682, #21229 ) ;
#14139 = LOCAL_TIME ( 14, 11, 27.00000000000000000, #3024 ) ;
#14140 = VERTEX_POINT ( 'NONE', #12061 ) ;
#14141 = DIRECTION ( 'NONE',  ( 0.000000000000000000, -1.000000000000000000, 2.081668171172168119E-15 ) ) ;
#14142 = AXIS2_PLACEMENT_3D ( 'NONE', #13886, #8430, #6772 ) ;
#14143 = DIRECTION ( 'NONE',  ( 0.000000000000000000, 0.000000000000000000, 1.000000000000000000 ) ) ;
#14144 = EDGE_LOOP ( 'NONE', ( #13922, #4242 ) ) ;
#14145 = VECTOR ( 'NONE', #20232, 1000.000000000000227 ) ;
#14146 = ADVANCED_FACE ( 'NONE', ( #982 ), #11955, .T. ) ;
#14147 = FACE_OUTER_BOUND ( 'NONE', #21241, .T. ) ;
#14148 = VECTOR ( 'NONE', #7763, 1000.000000000000114 ) ;
#14149 = DIRECTION ( 'NONE',  ( 0.9730401042858035643, -0.2306359803922028717, -5.959266323858677443E-17 ) ) ;
#14150 = CARTESIAN_POINT ( 'NONE',  ( -19.49999999982379961, -0.1021026942259700004, -8.658030917271079259E-14 ) ) ;
#14151 = ORIENTED_EDGE ( 'NONE', *, *, #20084, .F. ) ;
#14152 = DIRECTION ( 'NONE',  ( -0.9730401042858035643, 0.2306359803922028717, 5.958148513035547083E-17 ) ) ;
#14153 = APPROVAL ( #1523, 'UNKNOWN' ) ;
#14154 = APPROVAL_DATE_TIME ( #12279, #17382 ) ;
#14155 = ORIENTED_EDGE ( 'NONE', *, *, #5639, .F. ) ;
#14156 = CC_DESIGN_PERSON_AND_ORGANIZATION_ASSIGNMENT ( #509, #15352, ( #10633 ) ) ;
#14157 = VERTEX_POINT ( 'NONE', #4685 ) ;
#14158 = CARTESIAN_POINT ( 'NONE',  ( -19.49999999982360066, -0.1021026942259700004, 2.500000000000000000 ) ) ;
#14159 = CIRCLE ( 'NONE', #3543, 6.000000000000109246 ) ;
#14160 = COORDINATED_UNIVERSAL_TIME_OFFSET ( 0, 0, .AHEAD. ) ;
#14161 = CIRCLE ( 'NONE', #6974, 2.066999999999999726 ) ;
#14162 = EDGE_CURVE ( 'NONE', #815, #886, #4053, .T. ) ;
#14163 = CARTESIAN_POINT ( 'NONE',  ( -68.53146193154570653, -21.85922789657999843, -2.680796741387739937E-15 ) ) ;
#14164 = EDGE_CURVE ( 'NONE', #3332, #1138, #6342, .T. ) ;
#14165 = ORGANIZATION ( 'NAUO-ORG2', 'UNSPECIFIED', 'UNSPECIFIED' ) ;
#14166 = DIRECTION ( 'NONE',  ( 0.000000000000000000, -1.000000000000000000, 0.000000000000000000 ) ) ;
#14167 = AXIS2_PLACEMENT_3D ( 'NONE', #22364, #22807, #20257 ) ;
#14168 = TOROIDAL_SURFACE ( 'NONE', #3922, 2.700000000000000178, 0.2000000000000000111 ) ;
#14169 = AXIS2_PLACEMENT_3D ( 'NONE', #10880, #21880, #7640 ) ;
#14170 =( BOUNDED_CURVE ( )  B_SPLINE_CURVE ( 2, ( #12405, #19634, #3360 ),
 .UNSPECIFIED., .F., .F. ) 
 B_SPLINE_CURVE_WITH_KNOTS ( ( 3, 3 ),
 ( 0.000000000000000000, 0.08763271035584145607 ),
 .UNSPECIFIED. ) 
 CURVE ( )  GEOMETRIC_REPRESENTATION_ITEM ( )  RATIONAL_B_SPLINE_CURVE ( ( 1.000000000000000000, 1.077350269189623511, 1.077350269189624843 ) ) 
 REPRESENTATION_ITEM ( '' )  );
#14171 = DIRECTION ( 'NONE',  ( 0.000000000000000000, 0.000000000000000000, 1.000000000000000000 ) ) ;
#14172 = CARTESIAN_POINT ( 'NONE',  ( -19.89900739496031434, 14.70649742514172331, -5.842515507009584646E-15 ) ) ;
#14173 = PERSON_AND_ORGANIZATION ( #11966, #8758 ) ;
#14174 = DIRECTION ( 'NONE',  ( 1.138590270679730064E-14, 2.220446049251240387E-15, 1.000000000000000000 ) ) ;
#14175 = CARTESIAN_POINT ( 'NONE',  ( 34.40556712239430226, 8.514986143071229918, 27.68999999999999773 ) ) ;
#14176 = PLANE ( 'NONE',  #3656 ) ;
#14177 = EDGE_CURVE ( 'NONE', #13190, #17080, #16186, .T. ) ;
#14178 = CIRCLE ( 'NONE', #17219, 2.499999999999998668 ) ;
#14179 = CARTESIAN_POINT ( 'NONE',  ( 39.37089837072279863, 22.23982225285499936, -13.00000000000049916 ) ) ;
#14180 = EDGE_LOOP ( 'NONE', ( #22072, #13982, #6801, #11416, #5434 ) ) ;
#14181 = VECTOR ( 'NONE', #23040, 1000.000000000000000 ) ;
#14182 = CARTESIAN_POINT ( 'NONE',  ( -59.87132660632070014, -21.81388311970430038, 5.000000000000000000 ) ) ;
#14183 = UNCERTAINTY_MEASURE_WITH_UNIT (LENGTH_MEASURE( 1.000000000000000082E-05 ), #12086, 'distance_accuracy_value', 'NONE');
#14184 = PRODUCT_RELATED_PRODUCT_CATEGORY ( 'detail', '', ( #13107 ) ) ;
#14185 = CC_DESIGN_PERSON_AND_ORGANIZATION_ASSIGNMENT ( #9650, #22315, ( #22008 ) ) ;
#14186 = ORIENTED_EDGE ( 'NONE', *, *, #9085, .F. ) ;
#14187 = CARTESIAN_POINT ( 'NONE',  ( 37.37362508103680625, 25.08661566644159890, 13.00000000000000000 ) ) ;
#14188 = LINE ( 'NONE', #6604, #19705 ) ;
#14189 = ORIENTED_EDGE ( 'NONE', *, *, #10362, .F. ) ;
#14190 = EDGE_CURVE ( 'NONE', #2314, #20573, #15365, .T. ) ;
#14191 = DIRECTION ( 'NONE',  ( -3.210834492181040124E-17, 2.441916418604790135E-15, 1.000000000000000000 ) ) ;
#14192 = EDGE_CURVE ( 'NONE', #10599, #18495, #8998, .T. ) ;
#14193 = ORIENTED_EDGE ( 'NONE', *, *, #21382, .F. ) ;
#14194 = CARTESIAN_POINT ( 'NONE',  ( 35.59419854219520118, 9.774809681453278998, -26.30000000000050164 ) ) ;
#14195 = SHAPE_DEFINITION_REPRESENTATION ( #13494, #5348 ) ;
#14197 = CARTESIAN_POINT ( 'NONE',  ( 35.63933253682658631, 8.222551437987361211, 27.55602540378454535 ) ) ;
#14196 = PERSON ( 'NAUO-PER24', 'UNSPECIFIED', 'UNSPECIFIED', ('UNSPECIFIED'), ('UNSPECIFIED'), ('UNSPECIFIED') ) ;
#14198 = AXIS2_PLACEMENT_3D ( 'NONE', #736, #15247, #6235 ) ;
#14199 = CIRCLE ( 'NONE', #8138, 2.500000000000000444 ) ;
#14200 = CARTESIAN_POINT ( 'NONE',  ( -0.03403376487617889440, 6.499910899608420500, 2.500000000000090150 ) ) ;
#14201 = LINE ( 'NONE', #15972, #19650 ) ;
#14202 = DIRECTION ( 'NONE',  ( 1.000000000000000000, 0.000000000000000000, 0.000000000000000000 ) ) ;
#14203 = CARTESIAN_POINT ( 'NONE',  ( 36.15732495067950225, 25.37491064193190127, 13.00000000000000000 ) ) ;
#14204 = ORIENTED_EDGE ( 'NONE', *, *, #892, .T. ) ;
#14205 = DIRECTION ( 'NONE',  ( -0.2306359803922054252, -0.9730401042858028982, 0.000000000000000000 ) ) ;
#14206 = DESIGN_CONTEXT ( 'detailed design', #5333, 'design' ) ;
#14207 = ADVANCED_FACE ( 'NONE', ( #19176 ), #14052, .T. ) ;
#14208 = FACE_OUTER_BOUND ( 'NONE', #12833, .T. ) ;
#14209 = ORIENTED_EDGE ( 'NONE', *, *, #9702, .T. ) ;
#14210 = DIRECTION ( 'NONE',  ( -0.9997651245102161521, -0.02167246670483388357, 0.000000000000000000 ) ) ;
#14211 = PLANE ( 'NONE',  #22776 ) ;
#14212 = ORIENTED_EDGE ( 'NONE', *, *, #3915, .T. ) ;
#14213 = LINE ( 'NONE', #3281, #4329 ) ;
#14214 = VERTEX_POINT ( 'NONE', #1095 ) ;
#14215 = ORIENTED_EDGE ( 'NONE', *, *, #21811, .T. ) ;
#14216 = EDGE_CURVE ( 'NONE', #13906, #12652, #15598, .T. ) ;
#14217 = DATE_AND_TIME ( #16227, #4236 ) ;
#14218 = CARTESIAN_POINT ( 'NONE',  ( -2.500000000000000000, -17.30000000000000071, -2.500000000000000000 ) ) ;
#14219 = VERTEX_POINT ( 'NONE', #19401 ) ;
#14220 = EDGE_CURVE ( 'NONE', #7551, #23127, #15722, .T. ) ;
#14221 = CARTESIAN_POINT ( 'NONE',  ( -19.77176037304764833, 27.94687714311316284, 5.500000000004446221 ) ) ;
#14222 = PERSON_AND_ORGANIZATION_ROLE ( 'classification_officer' ) ;
#14223 = PRODUCT ( '1602p_c_20', '1602p_c_20', '', ( #18578 ) ) ;
#14224 = SECURITY_CLASSIFICATION_LEVEL ( 'unclassified' ) ;
#14225 = FACE_OUTER_BOUND ( 'NONE', #10470, .T. ) ;
#14226 = VECTOR ( 'NONE', #20758, 1000.000000000000114 ) ;
#14227 = CARTESIAN_POINT ( 'NONE',  ( -20.00000000000000000, -20.00000000000000000, -4.999999999995470290 ) ) ;
#14228 = ORIENTED_EDGE ( 'NONE', *, *, #8570, .T. ) ;
#14229 = ORIENTED_EDGE ( 'NONE', *, *, #5146, .T. ) ;
#14230 = DIRECTION ( 'NONE',  ( 0.9730401042858035643, -0.2306359803922028717, -5.959266323858677443E-17 ) ) ;
#14231 = DIRECTION ( 'NONE',  ( 0.2306359803922080620, 0.9730401042858023430, 2.536240390523813244E-14 ) ) ;
#14232 = ORIENTED_EDGE ( 'NONE', *, *, #21307, .F. ) ;
#14233 = APPROVAL ( #18908, 'UNSPECIFIED' ) ;
#14234 = FACE_OUTER_BOUND ( 'NONE', #1601, .T. ) ;
#14235 = LINE ( 'NONE', #20574, #3902 ) ;
#14236 = ORIENTED_EDGE ( 'NONE', *, *, #17909, .F. ) ;
#14237 = ORIENTED_EDGE ( 'NONE', *, *, #5597, .F. ) ;
#14238 = CALENDAR_DATE ( 2026, 31, 10 ) ;
#14239 = ORIENTED_EDGE ( 'NONE', *, *, #10708, .F. ) ;
#14240 = VERTEX_POINT ( 'NONE', #21295 ) ;
#14241 = DIRECTION ( 'NONE',  ( -1.751019220569994795E-16, -2.300154215587015208E-15, -1.000000000000000000 ) ) ;
#14242 = COORDINATED_UNIVERSAL_TIME_OFFSET ( 0, 0, .AHEAD. ) ;
#14243 = LINE ( 'NONE', #17706, #22590 ) ;
#14244 = APPROVAL_DATE_TIME ( #8791, #17350 ) ;
#14245 = EDGE_CURVE ( 'NONE', #11874, #6605, #13938, .T. ) ;
#14246 =( NAMED_UNIT ( * ) SI_UNIT ( $, .STERADIAN. ) SOLID_ANGLE_UNIT ( ) );
#14247 = DIRECTION ( 'NONE',  ( 0.000000000000000000, 0.000000000000000000, -1.000000000000000000 ) ) ;
#14248 = COORDINATED_UNIVERSAL_TIME_OFFSET ( 0, 0, .AHEAD. ) ;
#14249 =( GEOMETRIC_REPRESENTATION_CONTEXT ( 3 ) GLOBAL_UNCERTAINTY_ASSIGNED_CONTEXT ( ( #4917 ) ) GLOBAL_UNIT_ASSIGNED_CONTEXT ( ( #35, #1713, #23435 ) ) REPRESENTATION_CONTEXT ( 'NONE', 'WORKASPACE' ) );
#14250 = ORIENTED_EDGE ( 'NONE', *, *, #8601, .F. ) ;
#14251 = CARTESIAN_POINT ( 'NONE',  ( 53.10252809683457542, 27.27557781334508036, -2.066999999999924231 ) ) ;
#14252 = PLANE ( 'NONE',  #20004 ) ;
#14253 = VERTEX_POINT ( 'NONE', #10275 ) ;
#14254 = AXIS2_PLACEMENT_3D ( 'NONE', #6107, #4092, #394 ) ;
#14255 = DIRECTION ( 'NONE',  ( 0.000000000000000000, -1.000000000000000000, 2.081668171172168119E-15 ) ) ;
#14256 = DIRECTION ( 'NONE',  ( 1.000000000000000000, -1.466984912809909902E-16, 5.345529420184390105E-52 ) ) ;
#14257 = FACE_BOUND ( 'NONE', #14442, .T. ) ;
#14258 = ORIENTED_EDGE ( 'NONE', *, *, #23416, .T. ) ;
#14259 = ORIENTED_EDGE ( 'NONE', *, *, #17270, .F. ) ;
#14260 = CARTESIAN_POINT ( 'NONE',  ( -19.88588018851017125, 25.44948316784238074, 5.000000000004453327 ) ) ;
#14261 = APPROVAL_ROLE ( '' ) ;
#14262 = VERTEX_POINT ( 'NONE', #10051 ) ;
#14263 = ORIENTED_EDGE ( 'NONE', *, *, #8112, .T. ) ;
#14264 = CARTESIAN_POINT ( 'NONE',  ( 35.84667945578129888, -10.83917230622230043, -13.00000000000000000 ) ) ;
#14265 = CARTESIAN_POINT ( 'NONE',  ( 43.66832999130209458, 21.22121844545429781, -13.00000000000000000 ) ) ;
#14266 = CARTESIAN_POINT ( 'NONE',  ( 5.000000000000000000, -31.09999999999999787, -21.50000000000000000 ) ) ;
#14267 = PERSON_AND_ORGANIZATION ( #11966, #8758 ) ;
#14268 = DIRECTION ( 'NONE',  ( -0.9730401042858034533, 0.2306359803922031215, 0.000000000000000000 ) ) ;
#14269 = CIRCLE ( 'NONE', #18456, 1.749999999999998668 ) ;
#14270 = DIRECTION ( 'NONE',  ( 0.2306359803922028995, 0.9730401042858036753, -5.121148285185918258E-15 ) ) ;
#14271 = CIRCLE ( 'NONE', #16545, 3.500000000000000444 ) ;
#14272 = EDGE_CURVE ( 'NONE', #687, #15133, #22708, .T. ) ;
#14273 = CC_DESIGN_PERSON_AND_ORGANIZATION_ASSIGNMENT ( #9715, #7914, ( #13727 ) ) ;
#14274 = CARTESIAN_POINT ( 'NONE',  ( 33.72726576586480007, 23.57751093912980167, -13.00000000000030020 ) ) ;
#14275 = DATE_AND_TIME ( #7168, #13701 ) ;
#14276 = LINE ( 'NONE', #21516, #10271 ) ;
#14277 = CARTESIAN_POINT ( 'NONE',  ( -20.00000000397360012, 22.95208919256889857, -5.000000000000000000 ) ) ;
#14278 = APPLICATION_CONTEXT ( 'configuration controlled 3d designs of mechanical parts and assemblies' ) ;
#14279 = ADVANCED_FACE ( 'NONE', ( #21062 ), #5033, .F. ) ;
#14280 = EDGE_CURVE ( 'NONE', #21767, #15043, #1000, .T. ) ;
#14281 = CARTESIAN_POINT ( 'NONE',  ( 36.09092202081949807, 8.115512906978191054, -29.25000000000050093 ) ) ;
#14282 = VECTOR ( 'NONE', #10296, 1000.000000000000227 ) ;
#14283 = DIRECTION ( 'NONE',  ( 0.000000000000000000, 0.000000000000000000, 1.000000000000000000 ) ) ;
#14284 = AXIS2_PLACEMENT_3D ( 'NONE', #10626, #17854, #9297 ) ;
#14285 = VECTOR ( 'NONE', #19059, 1000.000000000000227 ) ;
#14286 = DIRECTION ( 'NONE',  ( 0.000000000000000000, -5.179188654504130612E-15, -1.000000000000000000 ) ) ;
#14287 = ORIENTED_EDGE ( 'NONE', *, *, #792, .F. ) ;
#14288 = DIRECTION ( 'NONE',  ( -0.000000000000000000, -0.000000000000000000, 1.000000000000000000 ) ) ;
#14289 = ORIENTED_EDGE ( 'NONE', *, *, #1567, .F. ) ;
#14290 = CARTESIAN_POINT ( 'NONE',  ( 35.59419854219520118, 9.774809681453278998, -26.88000000000049994 ) ) ;
#14291 = CARTESIAN_POINT ( 'NONE',  ( 113.9239269372040013, -8.791386740117969723, 3.438967838479089450E-14 ) ) ;
#14292 = ORIENTED_EDGE ( 'NONE', *, *, #23344, .F. ) ;
#14293 = CARTESIAN_POINT ( 'NONE',  ( -27.00000000000000000, -28.60000000000000142, -6.250000000000000000 ) ) ;
#14294 = EDGE_LOOP ( 'NONE', ( #11802, #22908 ) ) ;
#14295 = DIRECTION ( 'NONE',  ( 0.000000000000000000, 0.000000000000000000, 1.000000000000000000 ) ) ;
#14296 =( BOUNDED_CURVE ( )  B_SPLINE_CURVE ( 2, ( #6026, #13273, #4371 ),
 .UNSPECIFIED., .F., .F. ) 
 B_SPLINE_CURVE_WITH_KNOTS ( ( 3, 3 ),
 ( 0.000000000000000000, 0.2928548593876180162 ),
 .UNSPECIFIED. ) 
 CURVE ( )  GEOMETRIC_REPRESENTATION_ITEM ( )  RATIONAL_B_SPLINE_CURVE ( ( 1.000000000000000000, 1.037954849302039850, 1.000000000000000000 ) ) 
 REPRESENTATION_ITEM ( '' )  );
#14297 = VECTOR ( 'NONE', #20684, 1000.000000000000000 ) ;
#14298 = PERSON_AND_ORGANIZATION ( #2296, #7355 ) ;
#14299 = CARTESIAN_POINT ( 'NONE',  ( -58.40964484538829993, -25.30627767975780174, -2.500000000000000000 ) ) ;
#14300 = EDGE_CURVE ( 'NONE', #3018, #1694, #3243, .T. ) ;
#14301 = VECTOR ( 'NONE', #15589, 1000.000000000000227 ) ;
#14302 = VECTOR ( 'NONE', #12720, 999.9999999999998863 ) ;
#14303 = DIRECTION ( 'NONE',  ( 0.2306359803922031215, 0.9730401042858034533, -4.741332172907939802E-18 ) ) ;
#14304 = CC_DESIGN_PERSON_AND_ORGANIZATION_ASSIGNMENT ( #15650, #19328, ( #7318 ) ) ;
#14305 = CARTESIAN_POINT ( 'NONE',  ( 41.08211621068439712, 11.24883806106539907, -19.59999999999999787 ) ) ;
#14306 = CARTESIAN_POINT ( 'NONE',  ( 0.02181573787565703124, 0.1595291656146969883, -1.568993275710310442 ) ) ;
#14307 = CC_DESIGN_PERSON_AND_ORGANIZATION_ASSIGNMENT ( #21583, #11044, ( #8400 ) ) ;
#14308 = AXIS2_PLACEMENT_3D ( 'NONE', #2174, #9312, #262 ) ;
#14309 = CARTESIAN_POINT ( 'NONE',  ( 2.664535259100379799E-14, 6.659954201878760116E-16, 5.000000000000000000 ) ) ;
#14310 = CARTESIAN_POINT ( 'NONE',  ( -62.73971250800079957, -25.32895006819559924, -5.538452170245418869E-15 ) ) ;
#14311 = EDGE_CURVE ( 'NONE', #16214, #16298, #18091, .T. ) ;
#14312 = EDGE_CURVE ( 'NONE', #10583, #20142, #23004, .T. ) ;
#14313 = CARTESIAN_POINT ( 'NONE',  ( 13.56008835679158864, 17.12174078243637609, -3.470228899711813520E-15 ) ) ;
#14314 = CARTESIAN_POINT ( 'NONE',  ( -24.50000000000000000, -30.47499999999999787, 19.00000000000000000 ) ) ;
#14315 = CC_DESIGN_DATE_AND_TIME_ASSIGNMENT ( #13105, #2639, ( #14615 ) ) ;
#14316 = ORIENTED_EDGE ( 'NONE', *, *, #9384, .T. ) ;
#14317 = AXIS2_PLACEMENT_3D ( 'NONE', #16727, #18782, #13186 ) ;
#14318 = CARTESIAN_POINT ( 'NONE',  ( -20.00000000397270128, 22.95208919257349933, 5.500000000004459544 ) ) ;
#14319 = CARTESIAN_POINT ( 'NONE',  ( -20.00000000397430000, 22.95208919257349933, -6.749999999995570654 ) ) ;
#14320 = VERTEX_POINT ( 'NONE', #10625 ) ;
#14321 = AXIS2_PLACEMENT_3D ( 'NONE', #13388, #2575, #7921 ) ;
#14322 = AXIS2_PLACEMENT_3D ( 'NONE', #11818, #11705, #18824 ) ;
#14323 = DIRECTION ( 'NONE',  ( -1.000000000000000000, 0.000000000000000000, 0.000000000000000000 ) ) ;
#14324 = AXIS2_PLACEMENT_3D ( 'NONE', #17627, #1330, #867 ) ;
#14325 = ORIENTED_EDGE ( 'NONE', *, *, #2427, .F. ) ;
#14326 = VERTEX_POINT ( 'NONE', #8841 ) ;
#14327 = PERSON_AND_ORGANIZATION ( #11966, #8758 ) ;
#14328 = PLANE ( 'NONE',  #13373 ) ;
#14329 = ORIENTED_EDGE ( 'NONE', *, *, #14892, .F. ) ;
#14330 = LINE ( 'NONE', #21560, #21161 ) ;
#14331 = APPROVAL_STATUS ( 'not_yet_approved' ) ;
#14332 = AXIS2_PLACEMENT_3D ( 'NONE', #12898, #4224, #16924 ) ;
#14333 = EDGE_CURVE ( 'NONE', #7448, #21775, #5949, .T. ) ;
#14334 = DATE_TIME_ROLE ( 'classification_date' ) ;
#14335 = AXIS2_PLACEMENT_3D ( 'NONE', #15272, #22155, #5897 ) ;
#14336 = DIRECTION ( 'NONE',  ( -0.9999862922474493931, -0.005235963827110373843, 0.000000000000000000 ) ) ;
#14337 = EDGE_CURVE ( 'NONE', #17995, #19134, #17330, .T. ) ;
#14338 = CIRCLE ( 'NONE', #11331, 4.999999999999997335 ) ;
#14339 = ADVANCED_FACE ( 'NONE', ( #17853 ), #12852, .F. ) ;
#14340 = CONICAL_SURFACE ( 'NONE', #10196, 5.386751345948120218, 1.047197551196598297 ) ;
#14341 = CARTESIAN_POINT ( 'NONE',  ( 35.59419854219520118, 9.774809681453278998, -26.30000000000050164 ) ) ;
#14342 = ORIENTED_EDGE ( 'NONE', *, *, #9343, .T. ) ;
#14343 = PLANE ( 'NONE',  #1460 ) ;
#14344 = EDGE_CURVE ( 'NONE', #12306, #9018, #23302, .T. ) ;
#14345 = EDGE_CURVE ( 'NONE', #9613, #5079, #14396, .T. ) ;
#14346 = VERTEX_POINT ( 'NONE', #23414 ) ;
#14347 = DIRECTION ( 'NONE',  ( -0.9730401042858036753, 0.2306359803922031493, 5.432877459303543355E-17 ) ) ;
#14348 = CARTESIAN_POINT ( 'NONE',  ( -16.50000000000000000, -20.00000000000000000, 2.500000000000000000 ) ) ;
#14349 = CARTESIAN_POINT ( 'NONE',  ( -20.00000000000000000, -20.00000000000000000, -4.999999999995470290 ) ) ;
#14350 = ORIENTED_EDGE ( 'NONE', *, *, #9051, .T. ) ;
#14351 = CARTESIAN_POINT ( 'NONE',  ( -20.00000000000000000, -20.00000000000000000, 2.500000000000000000 ) ) ;
#14352 = CARTESIAN_POINT ( 'NONE',  ( 41.17437060284130013, 11.63805410277980101, 19.59999999999999787 ) ) ;
#14353 = ORIENTED_EDGE ( 'NONE', *, *, #22429, .F. ) ;
#14354 = ORIENTED_EDGE ( 'NONE', *, *, #1097, .F. ) ;
#14355 = SECURITY_CLASSIFICATION_LEVEL ( 'unclassified' ) ;
#14356 = ORIENTED_EDGE ( 'NONE', *, *, #352, .T. ) ;
#14357 = ORIENTED_EDGE ( 'NONE', *, *, #19019, .F. ) ;
#14358 = DIRECTION ( 'NONE',  ( 0.9730401042858035643, -0.2306359803922028717, -5.959266323858677443E-17 ) ) ;
#14359 = AXIS2_PLACEMENT_3D ( 'NONE', #4116, #11384, #11629 ) ;
#14360 = COORDINATED_UNIVERSAL_TIME_OFFSET ( 0, 0, .AHEAD. ) ;
#14361 = CARTESIAN_POINT ( 'NONE',  ( 13.92597371001594375, 15.97288132409727801, -3.408062879387094006E-15 ) ) ;
#14362 = PERSON_AND_ORGANIZATION_ROLE ( 'classification_officer' ) ;
#14363 = EDGE_CURVE ( 'NONE', #7703, #11043, #15945, .T. ) ;
#14364 = FACE_OUTER_BOUND ( 'NONE', #15750, .T. ) ;
#14365 = EDGE_CURVE ( 'NONE', #14375, #22099, #6727, .T. ) ;
#14366 = CALENDAR_DATE ( 2026, 31, 10 ) ;
#14367 = CLOSED_SHELL ( 'NONE', ( #20826, #8521, #14939, #7711, #8833, #3816, #16375, #12444, #6793, #10613, #19784, #12642, #193, #7377, #22222, #2809, #18864, #4568 ) ) ;
#14368 = ORIENTED_EDGE ( 'NONE', *, *, #13751, .T. ) ;
#14369 = DIRECTION ( 'NONE',  ( -3.974892857256893790E-34, -1.797095586565139883E-16, 1.000000000000000000 ) ) ;
#14370 = PLANE ( 'NONE',  #3691 ) ;
#14371 = ORIENTED_EDGE ( 'NONE', *, *, #5899, .F. ) ;
#14372 = CARTESIAN_POINT ( 'NONE',  ( 117.1241794131700118, -12.63305097454420078, -15.50000000000000000 ) ) ;
#14373 = FACE_OUTER_BOUND ( 'NONE', #1052, .T. ) ;
#14374 = DIRECTION ( 'NONE',  ( -2.982858504489139758E-17, 2.441916418604790135E-15, 1.000000000000000000 ) ) ;
#14375 = VERTEX_POINT ( 'NONE', #5254 ) ;
#14376 = VERTEX_POINT ( 'NONE', #8948 ) ;
#14378 = CARTESIAN_POINT ( 'NONE',  ( -69.82862846239015653, -8.365734848149525504, -7.200000000000000178 ) ) ;
#14377 = AXIS2_PLACEMENT_3D ( 'NONE', #19070, #9707, #18734 ) ;
#14379 = ORIENTED_EDGE ( 'NONE', *, *, #2945, .F. ) ;
#14380 = DATE_AND_TIME ( #7154, #10671 ) ;
#14381 = EDGE_CURVE ( 'NONE', #11110, #719, #7285, .T. ) ;
#14382 = ORIENTED_EDGE ( 'NONE', *, *, #18167, .T. ) ;
#14383 = ORIENTED_EDGE ( 'NONE', *, *, #20521, .F. ) ;
#14384 = DIRECTION ( 'NONE',  ( 0.000000000000000000, 0.000000000000000000, -1.000000000000000000 ) ) ;
#14385 = DIRECTION ( 'NONE',  ( -0.9730401042858035643, 0.2306359803922028717, 5.959266323858679908E-17 ) ) ;
#14386 = PLANE ( 'NONE',  #19913 ) ;
#14387 = SECURITY_CLASSIFICATION_LEVEL ( 'unclassified' ) ;
#14388 = DIRECTION ( 'NONE',  ( -0.9730401042858022320, 0.2306359803922080343, 5.959266323858941219E-17 ) ) ;
#14389 = CARTESIAN_POINT ( 'NONE',  ( 35.84667945578019754, -10.83917230622355987, 20.00000000000000000 ) ) ;
#14390 = CARTESIAN_POINT ( 'NONE',  ( 0.000000000000000000, 0.000000000000000000, 0.000000000000000000 ) ) ;
#14391 = APPROVAL_PERSON_ORGANIZATION ( #3907, #9960, #16257 ) ;
#14392 = AXIS2_PLACEMENT_3D ( 'NONE', #19760, #9428, #3717 ) ;
#14393 = CARTESIAN_POINT ( 'NONE',  ( -16.50000000000000000, -20.00000000000000711, 2.500000000000000000 ) ) ;
#14394 = PERSON_AND_ORGANIZATION ( #11966, #8758 ) ;
#14395 = DIRECTION ( 'NONE',  ( -0.2306359803922078400, -0.9730401042858023430, 5.204170427930423650E-15 ) ) ;
#14396 = LINE ( 'NONE', #17984, #16949 ) ;
#14397 = CARTESIAN_POINT ( 'NONE',  ( -19.99975861755289941, 22.95209442650110176, 2.499999999999950262 ) ) ;
#14398 = DIRECTION ( 'NONE',  ( 2.269747459788990007E-13, 2.220446049250330436E-15, 1.000000000000000000 ) ) ;
#14399 = DIRECTION ( 'NONE',  ( -0.7273594590164630391, 0.6862566701892800491, -3.364551046996708737E-15 ) ) ;
#14400 = ORIENTED_EDGE ( 'NONE', *, *, #4334, .F. ) ;
#14401 = CARTESIAN_POINT ( 'NONE',  ( 35.80298882477688949, 11.83572350794559114, 8.762640023735183803 ) ) ;
#14402 = EDGE_CURVE ( 'NONE', #23420, #11102, #13163, .T. ) ;
#14403 = EDGE_CURVE ( 'NONE', #19293, #8770, #12515, .T. ) ;
#14404 = PRODUCT_DEFINITION_SHAPE ( 'NONE', 'NONE',  #3051 ) ;
#14405 = ORIENTED_EDGE ( 'NONE', *, *, #14641, .T. ) ;
#14406 = CARTESIAN_POINT ( 'NONE',  ( 35.59419854219520118, 9.774809681453358934, -10.74538000000049998 ) ) ;
#14407 = FACE_OUTER_BOUND ( 'NONE', #22679, .T. ) ;
#14408 = CIRCLE ( 'NONE', #21968, 6.000000000000109246 ) ;
#14409 = ORIENTED_EDGE ( 'NONE', *, *, #4687, .T. ) ;
#14410 = AXIS2_PLACEMENT_3D ( 'NONE', #5580, #3453, #3683 ) ;
#14411 = DIRECTION ( 'NONE',  ( -0.9730401042858023430, 0.2306359803922080620, 5.959266323858944916E-17 ) ) ;
#14412 = ORIENTED_EDGE ( 'NONE', *, *, #14479, .T. ) ;
#14413 = CARTESIAN_POINT ( 'NONE',  ( 114.8178196092480050, -22.36345201740219935, 13.00000000000000000 ) ) ;
#14414 = APPROVAL_ROLE ( '' ) ;
#14415 = CARTESIAN_POINT ( 'NONE',  ( -28.52462712253550237, 6.350733138482030249, -0.7325259402521649976 ) ) ;
#14416 = VECTOR ( 'NONE', #21629, 1000.000000000000227 ) ;
#14417 = EDGE_CURVE ( 'NONE', #22099, #14375, #15821, .T. ) ;
#14418 = ADVANCED_FACE ( 'NONE', ( #12637 ), #16562, .T. ) ;
#14419 = DIRECTION ( 'NONE',  ( 0.9730401042858035643, -0.2306359803922028717, -5.958148513035547083E-17 ) ) ;
#14420 = FACE_OUTER_BOUND ( 'NONE', #7968, .T. ) ;
#14421 = DIRECTION ( 'NONE',  ( 1.000000000000000000, 0.000000000000000000, 0.000000000000000000 ) ) ;
#14422 = CC_DESIGN_APPROVAL ( #16346, ( #9386 ) ) ;
#14423 = APPROVAL_PERSON_ORGANIZATION ( #6587, #3641, #3125 ) ;
#14424 = CARTESIAN_POINT ( 'NONE',  ( -17.50000000000000000, -20.00000000000000000, 2.500000000000000000 ) ) ;
#14425 = CARTESIAN_POINT ( 'NONE',  ( 50.76434296088209663, 17.41090750189739822, 3.560102062092729998E-14 ) ) ;
#14426 = AXIS2_PLACEMENT_3D ( 'NONE', #9578, #8024, #16809 ) ;
#14427 = CARTESIAN_POINT ( 'NONE',  ( 50.90756547144185618, 18.01515514085710734, -2.066999999999964199 ) ) ;
#14428 = DESIGN_CONTEXT ( 'detailed design', #17476, 'design' ) ;
#14429 = ORIENTED_EDGE ( 'NONE', *, *, #15937, .F. ) ;
#14430 = CYLINDRICAL_SURFACE ( 'NONE', #508, 2.500000000000000444 ) ;
#14431 = CARTESIAN_POINT ( 'NONE',  ( 45.41807264205800010, 29.54199202163849947, -9.133960000000000079 ) ) ;
#14432 = AXIS2_PLACEMENT_3D ( 'NONE', #13552, #13802, #13669 ) ;
#14433 = ORIENTED_EDGE ( 'NONE', *, *, #125, .F. ) ;
#14434 = EDGE_CURVE ( 'NONE', #14944, #10793, #10994, .T. ) ;
#14435 = DIRECTION ( 'NONE',  ( 2.269747459788994803E-13, 2.220446049250330436E-15, 1.000000000000000000 ) ) ;
#14436 = SHAPE_REPRESENTATION ( '1602p_c_19', ( #12739 ), #11247 ) ;
#14437 = LINE ( 'NONE', #22022, #20870 ) ;
#14438 = ORIENTED_EDGE ( 'NONE', *, *, #709, .F. ) ;
#14440 = APPROVAL_STATUS ( 'not_yet_approved' ) ;
#14439 = APPROVAL ( #6644, 'UNKNOWN' ) ;
#14441 = CARTESIAN_POINT ( 'NONE',  ( 35.94015251278350576, 11.23436983788223209, 27.55602540378454179 ) ) ;
#14442 = EDGE_LOOP ( 'NONE', ( #17308, #15982 ) ) ;
#14443 = LOCAL_TIME ( 14, 11, 27.00000000000000000, #15705 ) ;
#14444 = CC_DESIGN_PERSON_AND_ORGANIZATION_ASSIGNMENT ( #11592, #2646, ( #6135 ) ) ;
#14445 = DIRECTION ( 'NONE',  ( -0.9730401042858024541, 0.2306359803922080898, 5.959266323858912869E-17 ) ) ;
#14446 = CC_DESIGN_APPROVAL ( #1881, ( #8384 ) ) ;
#14447 = PERSON_AND_ORGANIZATION_ROLE ( 'creator' ) ;
#14448 = EDGE_CURVE ( 'NONE', #2417, #18347, #19617, .T. ) ;
#14449 = ADVANCED_FACE ( 'NONE', ( #136 ), #21412, .T. ) ;
#14450 = AXIS2_PLACEMENT_3D ( 'NONE', #20740, #11746, #18624 ) ;
#14451 = CC_DESIGN_SECURITY_CLASSIFICATION ( #4974, ( #23514 ) ) ;
#14452 = ITEM_DEFINED_TRANSFORMATION ( 'NONE', 'NONE', #1887,  #12739 ) ;
#14453 = CARTESIAN_POINT ( 'NONE',  ( 35.59419854219520118, 9.774809681453278998, -26.30000000000050164 ) ) ;
#14454 = CIRCLE ( 'NONE', #12940, 5.000000000000000888 ) ;
#14455 = ADVANCED_BREP_SHAPE_REPRESENTATION ( '', ( #9448, #12739 ), #3642 ) ;
#14456 = DIRECTION ( 'NONE',  ( -0.5249589903860224505, 0.8511275218278915311, 1.187479569643817911E-16 ) ) ;
#14457 = ORIENTED_EDGE ( 'NONE', *, *, #12759, .T. ) ;
#14458 = DIRECTION ( 'NONE',  ( 0.005235963827110373843, -0.9999862922474493931, 0.000000000000000000 ) ) ;
#14459 = LOCAL_TIME ( 14, 11, 27.00000000000000000, #12921 ) ;
#14460 = EDGE_LOOP ( 'NONE', ( #18913, #13781, #10680, #454, #1458 ) ) ;
#14461 = PRODUCT_DEFINITION_FORMATION_WITH_SPECIFIED_SOURCE ( 'ANY', '', #5504, .NOT_KNOWN. ) ;
#14462 = DIRECTION ( 'NONE',  ( -0.1997366180463828189, -0.8426774492125620464, 0.5000000000000035527 ) ) ;
#14464 = VECTOR ( 'NONE', #13423, 1000.000000000000000 ) ;
#14463 = LINE ( 'NONE', #5203, #11080 ) ;
#14465 = DIRECTION ( 'NONE',  ( -1.466984912809907930E-16, -2.805478249466190329E-20, -1.000000000000000000 ) ) ;
#14466 = ORIENTED_EDGE ( 'NONE', *, *, #7667, .F. ) ;
#14467 = EDGE_CURVE ( 'NONE', #17514, #1281, #22485, .T. ) ;
#14468 = DIRECTION ( 'NONE',  ( -0.9730401042858035643, 0.2306359803922028717, 6.126766849694256332E-17 ) ) ;
#14469 = CARTESIAN_POINT ( 'NONE',  ( -28.95596696049959817, -6.651703575491109355, 4.767474059747909720 ) ) ;
#14470 = LOCAL_TIME ( 14, 11, 27.00000000000000000, #8414 ) ;
#14471 = APPLICATION_CONTEXT ( 'configuration controlled 3d designs of mechanical parts and assemblies' ) ;
#14472 = ORIENTED_EDGE ( 'NONE', *, *, #2450, .F. ) ;
#14473 = APPROVAL_ROLE ( '' ) ;
#14474 = ORIENTED_EDGE ( 'NONE', *, *, #18006, .F. ) ;
#14475 = ORIENTED_EDGE ( 'NONE', *, *, #13591, .F. ) ;
#14476 = PLANE ( 'NONE',  #17559 ) ;
#14477 = DATE_TIME_ROLE ( 'creation_date' ) ;
#14478 = ADVANCED_FACE ( 'NONE', ( #23179 ), #6946, .F. ) ;
#14479 = EDGE_CURVE ( 'NONE', #4801, #3898, #16756, .T. ) ;
#14480 = LOCAL_TIME ( 14, 11, 27.00000000000000000, #4834 ) ;
#14481 = CYLINDRICAL_SURFACE ( 'NONE', #22210, 4.099999999999999645 ) ;
#14482 = DATE_AND_TIME ( #7371, #7200 ) ;
#14483 = DIRECTION ( 'NONE',  ( -6.662161100567945949E-09, 1.000000000000000000, -2.081668171172169697E-15 ) ) ;
#14484 = AXIS2_PLACEMENT_3D ( 'NONE', #4690, #22954, #17280 ) ;
#14485 = APPROVAL_PERSON_ORGANIZATION ( #17173, #15592, #18491 ) ;
#14486 = CARTESIAN_POINT ( 'NONE',  ( 45.07211867146960316, 28.08243186520980217, -10.02499999999999858 ) ) ;
#14487 = COORDINATED_UNIVERSAL_TIME_OFFSET ( 0, 0, .AHEAD. ) ;
#14488 = ORIENTED_EDGE ( 'NONE', *, *, #1114, .T. ) ;
#14489 = CARTESIAN_POINT ( 'NONE',  ( 35.59419854219520118, 9.774809681453550780, 27.18999999999999773 ) ) ;
#14490 = VERTEX_POINT ( 'NONE', #9776 ) ;
#14491 = EDGE_CURVE ( 'NONE', #7204, #20882, #2405, .T. ) ;
#14492 = LOCAL_TIME ( 14, 11, 27.00000000000000000, #8473 ) ;
#14493 = DIRECTION ( 'NONE',  ( 0.9730401042858024541, -0.2306359803922080898, -5.959266323858942451E-17 ) ) ;
#14494 = CARTESIAN_POINT ( 'NONE',  ( -62.91413607658799378, 7.983193290926558383, 2.191364059223300011E-15 ) ) ;
#14495 = DIRECTION ( 'NONE',  ( 4.758660364968300250E-15, 2.033490192229560220E-14, -1.000000000000000000 ) ) ;
#14496 = ORIENTED_EDGE ( 'NONE', *, *, #5431, .T. ) ;
#14497 = ORIENTED_EDGE ( 'NONE', *, *, #18074, .F. ) ;
#14498 = DIRECTION ( 'NONE',  ( -2.269747459788999852E-13, -2.220446049250325308E-15, -1.000000000000000000 ) ) ;
#14499 = VECTOR ( 'NONE', #4006, 1000.000000000000000 ) ;
#14500 = ORIENTED_EDGE ( 'NONE', *, *, #6971, .T. ) ;
#14501 = AXIS2_PLACEMENT_3D ( 'NONE', #21096, #22985, #3046 ) ;
#14502 = COORDINATED_UNIVERSAL_TIME_OFFSET ( 0, 0, .AHEAD. ) ;
#14503 = ORIENTED_EDGE ( 'NONE', *, *, #4181, .F. ) ;
#14504 = AXIS2_PLACEMENT_3D ( 'NONE', #1020, #11530, #18767 ) ;
#14505 = ORIENTED_EDGE ( 'NONE', *, *, #1852, .F. ) ;
#14506 = AXIS2_PLACEMENT_3D ( 'NONE', #3515, #16444, #16217 ) ;
#14507 = CARTESIAN_POINT ( 'NONE',  ( -14.00000000144900092, -4.350228928435750042, -6.749999999996870059 ) ) ;
#14508 = CC_DESIGN_SECURITY_CLASSIFICATION ( #1214, ( #23511 ) ) ;
#14509 = CARTESIAN_POINT ( 'NONE',  ( -26.99999999999959854, -33.09999999999999432, 25.00000000000000000 ) ) ;
#14510 = MECHANICAL_CONTEXT ( 'NONE', #4574, 'mechanical' ) ;
#14511 = EDGE_CURVE ( 'NONE', #1934, #19462, #13452, .T. ) ;
#14512 = CARTESIAN_POINT ( 'NONE',  ( 45.41807264205800010, 29.54199202163849947, 9.133960000000000079 ) ) ;
#14513 = VECTOR ( 'NONE', #11099, 1000.000000000000000 ) ;
#14514 = EDGE_CURVE ( 'NONE', #15793, #12809, #22332, .T. ) ;
#14515 = LINE ( 'NONE', #3938, #17851 ) ;
#14516 = AXIS2_PLACEMENT_3D ( 'NONE', #6414, #19143, #10011 ) ;
#14517 = CC_DESIGN_SECURITY_CLASSIFICATION ( #17927, ( #8830 ) ) ;
#14518 = CARTESIAN_POINT ( 'NONE',  ( 0.000000000000000000, 0.000000000000000000, 0.000000000000000000 ) ) ;
#14519 = VECTOR ( 'NONE', #7096, 1000.000000000000000 ) ;
#14520 = ORIENTED_EDGE ( 'NONE', *, *, #17707, .T. ) ;
#14521 = PLANE ( 'NONE',  #10586 ) ;
#14522 = PERSON_AND_ORGANIZATION ( #11966, #8758 ) ;
#14523 = VECTOR ( 'NONE', #22726, 999.9999999999998863 ) ;
#14524 = DIRECTION ( 'NONE',  ( -1.524428182562999945E-15, -6.173091865707990781E-15, -1.000000000000000000 ) ) ;
#14525 = DIRECTION ( 'NONE',  ( 0.000000000000000000, 0.000000000000000000, -1.000000000000000000 ) ) ;
#14526 = DIRECTION ( 'NONE',  ( 0.000000000000000000, -1.000000000000000000, 5.551115123125781913E-15 ) ) ;
#14527 = CARTESIAN_POINT ( 'NONE',  ( -58.53873997113881700, 12.69366727667581429, 3.427095671567204722E-15 ) ) ;
#14528 = CARTESIAN_POINT ( 'NONE',  ( 34.40556712239430226, 8.514986143071238800, 29.25000000000000000 ) ) ;
#14529 = ORIENTED_EDGE ( 'NONE', *, *, #13522, .T. ) ;
#14530 = VECTOR ( 'NONE', #7137, 1000.000000000000000 ) ;
#14531 = CARTESIAN_POINT ( 'NONE',  ( 33.65811390067847242, 10.51125079953912334, 8.996926784497372154 ) ) ;
#14532 = AXIS2_PLACEMENT_3D ( 'NONE', #20416, #15532, #19118 ) ;
#14533 = CC_DESIGN_PERSON_AND_ORGANIZATION_ASSIGNMENT ( #9080, #7311, ( #4231 ) ) ;
#14534 = PRODUCT_DEFINITION_FORMATION_WITH_SPECIFIED_SOURCE ( 'ANY', '', #7796, .NOT_KNOWN. ) ;
#14535 = ORIENTED_EDGE ( 'NONE', *, *, #21135, .F. ) ;
#14536 = CYLINDRICAL_SURFACE ( 'NONE', #3535, 2.500000000000000888 ) ;
#14537 = PLANE ( 'NONE',  #2248 ) ;
#14538 = ORIENTED_EDGE ( 'NONE', *, *, #11506, .T. ) ;
#14539 = CONICAL_SURFACE ( 'NONE', #7342, 2.283500000000000085, 0.7853981633974447263 ) ;
#14540 = AXIS2_PLACEMENT_3D ( 'NONE', #12755, #7295, #16299 ) ;
#14541 = DIRECTION ( 'NONE',  ( 0.9730401042858035643, -0.2306359803922028717, -5.959266323858677443E-17 ) ) ;
#14542 = ORIENTED_EDGE ( 'NONE', *, *, #21001, .F. ) ;
#14543 = AXIS2_PLACEMENT_3D ( 'NONE', #23473, #23295, #3466 ) ;
#14544 = CARTESIAN_POINT ( 'NONE',  ( 114.8178196092480050, -22.36345201740219935, -20.00000000000000000 ) ) ;
#14545 = DATE_AND_TIME ( #16308, #11545 ) ;
#14546 = DIRECTION ( 'NONE',  ( 0.9730401042858032312, -0.2306359803922040375, 1.121193430162474340E-15 ) ) ;
#14547 = VECTOR ( 'NONE', #2180, 1000.000000000000000 ) ;
#14548 = LINE ( 'NONE', #16313, #9631 ) ;
#14549 = EDGE_CURVE ( 'NONE', #5883, #16045, #15051, .T. ) ;
#14550 = DIRECTION ( 'NONE',  ( 0.8511275218278916421, 0.5249589903860222284, 1.038675759242784740E-16 ) ) ;
#14551 = CARTESIAN_POINT ( 'NONE',  ( 0.000000000000000000, 0.000000000000000000, 0.000000000000000000 ) ) ;
#14552 = ORGANIZATION ( 'NAUO-ORG3', 'UNSPECIFIED', 'UNSPECIFIED' ) ;
#14553 = VECTOR ( 'NONE', #16236, 1000.000000000000114 ) ;
#14554 = DIRECTION ( 'NONE',  ( 0.000000000000000000, 0.000000000000000000, 1.000000000000000000 ) ) ;
#14555 = AXIS2_PLACEMENT_3D ( 'NONE', #16043, #1663, #13913 ) ;
#14556 = CARTESIAN_POINT ( 'NONE',  ( -27.00000000000000000, -31.09999999999999787, -19.00000000000000000 ) ) ;
#14557 = CARTESIAN_POINT ( 'NONE',  ( 53.20239347634440463, 27.69690417850090114, 3.288194835581189691E-14 ) ) ;
#14558 = AXIS2_PLACEMENT_3D ( 'NONE', #9965, #11392, #9611 ) ;
#14559 = DIRECTION ( 'NONE',  ( -6.662112528310618598E-09, 1.000000000000000000, -2.220444537147720967E-15 ) ) ;
#14560 = CARTESIAN_POINT ( 'NONE',  ( -20.11411981943522775, 20.45469521730081652, 5.500000000004466649 ) ) ;
#14561 = DIRECTION ( 'NONE',  ( 1.213490492418603984E-15, 4.861311874477930828E-15, 1.000000000000000000 ) ) ;
#14562 = ORIENTED_EDGE ( 'NONE', *, *, #18926, .T. ) ;
#14563 = ORIENTED_EDGE ( 'NONE', *, *, #7639, .T. ) ;
#14564 = DIRECTION ( 'NONE',  ( -0.2306359803922033158, -0.9730401042858034533, 0.000000000000000000 ) ) ;
#14565 = CARTESIAN_POINT ( 'NONE',  ( -19.77176037304765188, 27.94687714311316640, 5.000000000004446221 ) ) ;
#14566 = ORIENTED_EDGE ( 'NONE', *, *, #2082, .F. ) ;
#14567 = PERSON_AND_ORGANIZATION_ROLE ( 'creator' ) ;
#14568 = CARTESIAN_POINT ( 'NONE',  ( -69.90454993788326021, 6.134066389438223688, -5.500000000000079048 ) ) ;
#14569 = AXIS2_PLACEMENT_3D ( 'NONE', #9566, #392, #11713 ) ;
#14570 = ORIENTED_EDGE ( 'NONE', *, *, #17214, .F. ) ;
#14571 = PLANE ( 'NONE',  #7891 ) ;
#14572 = PERSON_AND_ORGANIZATION ( #11966, #8758 ) ;
#14573 = AXIS2_PLACEMENT_3D ( 'NONE', #5827, #457, #12830 ) ;
#14574 = SECURITY_CLASSIFICATION_LEVEL ( 'unclassified' ) ;
#14575 = DIRECTION ( 'NONE',  ( -0.9730401042858024541, 0.2306359803922080898, 5.959266323858942451E-17 ) ) ;
#14576 = ADVANCED_FACE ( 'NONE', ( #491 ), #18564, .T. ) ;
#14577 = DIRECTION ( 'NONE',  ( -6.123230174520380038E-17, -4.962644601432250805E-15, -1.000000000000000000 ) ) ;
#14578 = ORIENTED_EDGE ( 'NONE', *, *, #6086, .T. ) ;
#14579 = CARTESIAN_POINT ( 'NONE',  ( 117.1241794131700118, -12.63305097454420078, -15.50000000000000000 ) ) ;
#14580 = APPROVAL ( #20029, 'UNKNOWN' ) ;
#14581 = EDGE_LOOP ( 'NONE', ( #4183, #7403, #15426, #8531 ) ) ;
#14582 =( BOUNDED_CURVE ( )  B_SPLINE_CURVE ( 2, ( #22324, #13790, #2506 ),
 .UNSPECIFIED., .F., .F. ) 
 B_SPLINE_CURVE_WITH_KNOTS ( ( 3, 3 ),
 ( 0.2928548593876180162, 0.5857097187752370315 ),
 .UNSPECIFIED. ) 
 CURVE ( )  GEOMETRIC_REPRESENTATION_ITEM ( )  RATIONAL_B_SPLINE_CURVE ( ( 1.000000000000000000, 1.037954849302049842, 1.000000000000000000 ) ) 
 REPRESENTATION_ITEM ( '' )  );
#14583 = DIRECTION ( 'NONE',  ( -0.9730401042858036753, 0.2306359803922028995, -2.804983810440358801E-16 ) ) ;
#14584 = FACE_BOUND ( 'NONE', #16357, .T. ) ;
#14585 = FACE_OUTER_BOUND ( 'NONE', #8022, .T. ) ;
#14586 = VERTEX_POINT ( 'NONE', #22106 ) ;
#14587 = ADVANCED_FACE ( 'NONE', ( #11338, #2156 ), #6073, .F. ) ;
#14588 = EDGE_CURVE ( 'NONE', #22882, #10807, #22215, .T. ) ;
#14589 = COORDINATED_UNIVERSAL_TIME_OFFSET ( 0, 0, .AHEAD. ) ;
#14590 = DIRECTION ( 'NONE',  ( -0.9997651245102238127, -0.02167246670447303680, 0.000000000000000000 ) ) ;
#14591 = EDGE_LOOP ( 'NONE', ( #12225, #11074, #12342, #10082 ) ) ;
#14592 = APPROVAL_ROLE ( '' ) ;
#14593 = ORIENTED_EDGE ( 'NONE', *, *, #7120, .F. ) ;
#14594 = ORIENTED_EDGE ( 'NONE', *, *, #13660, .F. ) ;
#14595 = CARTESIAN_POINT ( 'NONE',  ( -20.00000000000000000, -20.00000000000000000, -2.500000000000000000 ) ) ;
#14596 = MECHANICAL_CONTEXT ( 'NONE', #473, 'mechanical' ) ;
#14597 = DIRECTION ( 'NONE',  ( 1.000000000000000000, -1.751019220569989865E-16, -7.006492321624090605E-47 ) ) ;
#14598 = CALENDAR_DATE ( 2026, 31, 10 ) ;
#14599 = CARTESIAN_POINT ( 'NONE',  ( -0.03653820904332859970, 20.46006235366549575, 4.500000000000000000 ) ) ;
#14600 = AXIS2_PLACEMENT_3D ( 'NONE', #10450, #6388, #9975 ) ;
#14601 = EDGE_CURVE ( 'NONE', #8501, #252, #22458, .T. ) ;
#14602 = CARTESIAN_POINT ( 'NONE',  ( -68.53146193154570653, -21.85922789657999843, -2.680796741387739937E-15 ) ) ;
#14603 = CC_DESIGN_PERSON_AND_ORGANIZATION_ASSIGNMENT ( #6151, #11401, ( #6551 ) ) ;
#14604 = PERSON_AND_ORGANIZATION_ROLE ( 'classification_officer' ) ;
#14605 = PRODUCT ( '1602p_c_04', '1602p_c_04', '', ( #8294 ) ) ;
#14606 = PRODUCT_RELATED_PRODUCT_CATEGORY ( 'detail', '', ( #15730 ) ) ;
#14607 = VERTEX_POINT ( 'NONE', #7519 ) ;
#14608 = DIRECTION ( 'NONE',  ( -0.1997366180463773788, -0.8426774492125681526, -0.4999999999999950595 ) ) ;
#14609 = ORIENTED_EDGE ( 'NONE', *, *, #11620, .F. ) ;
#14610 = EDGE_CURVE ( 'NONE', #12435, #6022, #15413, .T. ) ;
#14611 = B_SPLINE_CURVE_WITH_KNOTS ( 'NONE', 3,
 ( #16189, #7176, #14401, #18335, #21638, #5380, #1808, #3605, #10874, #16295, #18, #7292, #17861, #14531, #7524, #5612, #21769, #5503, #12752, #12980, #1924, #9183, #16418, #20228, #144, #21874, #2054, #9301 ),
 .UNSPECIFIED., .F., .F.,
 ( 4, 2, 2, 2, 2, 2, 2, 2, 2, 2, 2, 2, 2, 4 ),
 ( 0.000000000000000000, 0.0004072576943254697392, 0.0008145153886509394784, 0.001629030777301878957, 0.002036288471627348967, 0.002443546165952819194, 0.002850803860278289421, 0.003258061554603759648, 0.004072576943254694465, 0.004479834637580166860, 0.004887092331905638389, 0.005294350026231110784, 0.005701607720556582312, 0.006516123109207543583 ),
 .UNSPECIFIED. ) ;
#14612 = EDGE_CURVE ( 'NONE', #18104, #7299, #5190, .T. ) ;
#14613 = CARTESIAN_POINT ( 'NONE',  ( -14.00000000000000000, -19.99999999944489915, 8.000000000004488854 ) ) ;
#14614 = CIRCLE ( 'NONE', #19922, 2.500000000000001332 ) ;
#14615 = PRODUCT_DEFINITION ( 'UNKNOWN', '', #14812, #17770 ) ;
#14616 = CARTESIAN_POINT ( 'NONE',  ( 36.57467860885130051, 21.71590586959139912, 15.00000000000000000 ) ) ;
#14617 = DIRECTION ( 'NONE',  ( -0.7071067811865475727, 0.000000000000000000, -0.7071067811865475727 ) ) ;
#14618 = ORIENTED_EDGE ( 'NONE', *, *, #7805, .F. ) ;
#14619 = VERTEX_POINT ( 'NONE', #2515 ) ;
#14620 = CARTESIAN_POINT ( 'NONE',  ( -14.98746859792130159, 26.70208920133150343, -6.749999999996710187 ) ) ;
#14621 = ORIENTED_EDGE ( 'NONE', *, *, #1963, .F. ) ;
#14622 = PERSON_AND_ORGANIZATION_ROLE ( 'classification_officer' ) ;
#14623 = ORIENTED_EDGE ( 'NONE', *, *, #7316, .T. ) ;
#14624 = VERTEX_POINT ( 'NONE', #11452 ) ;
#14625 = DIRECTION ( 'NONE',  ( 2.982858504577314686E-17, -2.441916418604790135E-15, -1.000000000000000000 ) ) ;
#14626 = LINE ( 'NONE', #16740, #16869 ) ;
#14627 = APPLICATION_PROTOCOL_DEFINITION ( 'international standard', 'config_control_design', 1994, #18712 ) ;
#14628 = CARTESIAN_POINT ( 'NONE',  ( 28.89837840081079889, -1.998294948772169954, 13.00000000000019895 ) ) ;
#14629 = DIRECTION ( 'NONE',  ( 2.979589986992270586E-09, -0.4472135954999619800, 0.8944271909999139680 ) ) ;
#14630 = EDGE_CURVE ( 'NONE', #12948, #3328, #7862, .T. ) ;
#14631 = EDGE_LOOP ( 'NONE', ( #2704, #2664 ) ) ;
#14632 = AXIS2_PLACEMENT_3D ( 'NONE', #11004, #276, #8875 ) ;
#14633 = CARTESIAN_POINT ( 'NONE',  ( -59.87132660632070014, -21.81388311970430038, 5.000000000000000000 ) ) ;
#14634 = DATE_AND_TIME ( #3811, #20161 ) ;
#14635 = ORIENTED_EDGE ( 'NONE', *, *, #17547, .T. ) ;
#14636 = CARTESIAN_POINT ( 'NONE',  ( -20.00000000000000000, -22.50000000000000000, -4.999999999995464961 ) ) ;
#14637 = DIRECTION ( 'NONE',  ( 1.217822455144494161E-14, 0.000000000000000000, 1.000000000000000000 ) ) ;
#14638 = EDGE_CURVE ( 'NONE', #22508, #21478, #18880, .T. ) ;
#14639 = LINE ( 'NONE', #18086, #9357 ) ;
#14640 = CARTESIAN_POINT ( 'NONE',  ( -17.00058775598304095, -0.04789535763852829919, -5.000000000000000000 ) ) ;
#14641 = EDGE_CURVE ( 'NONE', #7551, #16084, #9400, .T. ) ;
#14642 = FACE_OUTER_BOUND ( 'NONE', #849, .T. ) ;
#14643 = EDGE_LOOP ( 'NONE', ( #2225, #18343, #7150, #6262 ) ) ;
#14644 = CARTESIAN_POINT ( 'NONE',  ( 46.46175228317039796, -6.161274394849590053, -13.00000000000000000 ) ) ;
#14645 = UNCERTAINTY_MEASURE_WITH_UNIT (LENGTH_MEASURE( 1.000000000000000082E-05 ), #20005, 'distance_accuracy_value', 'NONE');
#14646 = ORIENTED_EDGE ( 'NONE', *, *, #12136, .T. ) ;
#14647 = FACE_OUTER_BOUND ( 'NONE', #22686, .T. ) ;
#14648 = FACE_OUTER_BOUND ( 'NONE', #20266, .T. ) ;
#14649 = VERTEX_POINT ( 'NONE', #11092 ) ;
#14650 = CARTESIAN_POINT ( 'NONE',  ( -65.62876257020761273, -24.89748912807110059, -5.000000000000000000 ) ) ;
#14651 = AXIS2_PLACEMENT_3D ( 'NONE', #1416, #5112, #7134 ) ;
#14652 = VERTEX_POINT ( 'NONE', #2046 ) ;
#14653 = CARTESIAN_POINT ( 'NONE',  ( 97.29330225143137056, -16.08541248458771022, 13.00000000000000000 ) ) ;
#14654 = PERSON_AND_ORGANIZATION_ROLE ( 'classification_officer' ) ;
#14655 = LINE ( 'NONE', #22001, #21889 ) ;
#14656 =( LENGTH_UNIT ( ) NAMED_UNIT ( * ) SI_UNIT ( .MILLI., .METRE. ) );
#14657 = DIRECTION ( 'NONE',  ( 0.000000000000000000, 0.000000000000000000, 1.000000000000000000 ) ) ;
#14658 = DIRECTION ( 'NONE',  ( -0.9997651245102240347, -0.02167246670447264822, 0.000000000000000000 ) ) ;
#14659 = VECTOR ( 'NONE', #15044, 1000.000000000000000 ) ;
#14660 = AXIS2_PLACEMENT_3D ( 'NONE', #9806, #11717, #4210 ) ;
#14661 = DIRECTION ( 'NONE',  ( -1.000000000000000000, 0.000000000000000000, 0.000000000000000000 ) ) ;
#14662 = CARTESIAN_POINT ( 'NONE',  ( 2.500000000000000000, 3.061616997868383141E-16, -2.500000000000000000 ) ) ;
#14663 = CARTESIAN_POINT ( 'NONE',  ( -20.00000000397459843, 22.95208919257349933, -7.999999999995569766 ) ) ;
#14664 = CARTESIAN_POINT ( 'NONE',  ( 113.2956221386590130, -28.78551670568859677, -2.700000000000000178 ) ) ;
#14665 = DIRECTION ( 'NONE',  ( 0.2306359803922031215, 0.9730401042858033422, -4.741332172907962143E-18 ) ) ;
#14666 = ORIENTED_EDGE ( 'NONE', *, *, #13892, .T. ) ;
#14667 = ORIENTED_EDGE ( 'NONE', *, *, #15363, .F. ) ;
#14668 = CARTESIAN_POINT ( 'NONE',  ( -3.458317987535629801, 19.03127855354509990, -7.892745253163399067E-16 ) ) ;
#14669 = DIRECTION ( 'NONE',  ( 0.9730401042858024541, -0.2306359803922080898, -5.959266323858852472E-17 ) ) ;
#14670 = AXIS2_PLACEMENT_3D ( 'NONE', #5256, #7061, #3708 ) ;
#14671 = ORIENTED_EDGE ( 'NONE', *, *, #20871, .F. ) ;
#14672 = DIRECTION ( 'NONE',  ( 1.000000000000000000, 3.099353312215988811E-62, 0.000000000000000000 ) ) ;
#14673 = ADVANCED_FACE ( 'NONE', ( #9296 ), #16521, .F. ) ;
#14674 = VERTEX_POINT ( 'NONE', #5715 ) ;
#14675 = VECTOR ( 'NONE', #8033, 1000.000000000000000 ) ;
#14676 = CARTESIAN_POINT ( 'NONE',  ( -62.74088165156670271, -25.10566213532069924, -5.538319619822460249E-15 ) ) ;
#14677 = AXIS2_PLACEMENT_3D ( 'NONE', #5850, #18685, #4310 ) ;
#14678 = APPROVAL_STATUS ( 'not_yet_approved' ) ;
#14679 = CARTESIAN_POINT ( 'NONE',  ( 66.60056952104010008, 2.425487965306460048, 1.173314102775059961E-14 ) ) ;
#14680 = ITEM_DEFINED_TRANSFORMATION ( 'NONE', 'NONE', #17301,  #12739 ) ;
#14681 = VECTOR ( 'NONE', #10043, 1000.000000000000000 ) ;
#14682 = DIRECTION ( 'NONE',  ( 0.000000000000000000, 0.000000000000000000, 1.000000000000000000 ) ) ;
#14683 = ORIENTED_EDGE ( 'NONE', *, *, #15661, .F. ) ;
#14684 = AXIS2_PLACEMENT_3D ( 'NONE', #11339, #9419, #9780 ) ;
#14685 = CARTESIAN_POINT ( 'NONE',  ( -32.65701080836369385, 9.273987487686079945, -2.500000000000000000 ) ) ;
#14686 = EDGE_LOOP ( 'NONE', ( #22341, #2615, #15762, #20110 ) ) ;
#14687 = CARTESIAN_POINT ( 'NONE',  ( -19.49999999982519938, -0.1021026942257829973, -2.500000000000000000 ) ) ;
#14688 = VECTOR ( 'NONE', #22521, 999.9999999999998863 ) ;
#14689 = CONICAL_SURFACE ( 'NONE', #11299, 2.283499999999998753, 0.7853981633974433940 ) ;
#14690 = AXIS2_PLACEMENT_3D ( 'NONE', #21728, #106, #23274 ) ;
#14691 = ORIENTED_EDGE ( 'NONE', *, *, #10362, .T. ) ;
#14692 = DIRECTION ( 'NONE',  ( 1.138590270679734009E-14, 2.220446049251240387E-15, 1.000000000000000000 ) ) ;
#14693 = LINE ( 'NONE', #20829, #1586 ) ;
#14694 = CARTESIAN_POINT ( 'NONE',  ( 114.2412296582679971, -24.79605227811670076, -2.999999999999940048 ) ) ;
#14695 = EDGE_LOOP ( 'NONE', ( #18887, #9008, #9341, #19427 ) ) ;
#14696 = COORDINATED_UNIVERSAL_TIME_OFFSET ( 0, 0, .AHEAD. ) ;
#14697 = DIRECTION ( 'NONE',  ( 0.005235964011411635595, -0.9999862922464843873, 2.602085213965213008E-15 ) ) ;
#14698 = ORIENTED_EDGE ( 'NONE', *, *, #17072, .F. ) ;
#14699 = APPROVAL_ROLE ( '' ) ;
#14700 = EDGE_CURVE ( 'NONE', #5938, #2368, #2179, .T. ) ;
#14701 = ORIENTED_EDGE ( 'NONE', *, *, #9271, .T. ) ;
#14702 = ORIENTED_EDGE ( 'NONE', *, *, #8767, .F. ) ;
#14703 = DIRECTION ( 'NONE',  ( 5.964507377817269296E-17, 4.861311874385510251E-15, 1.000000000000000000 ) ) ;
#14704 = DATE_AND_TIME ( #20049, #22073 ) ;
#14705 = AXIS2_PLACEMENT_3D ( 'NONE', #11855, #6735, #1126 ) ;
#14706 = DIRECTION ( 'NONE',  ( 0.1177891644214619504, 0.4969457958705769118, 0.8597503060257977170 ) ) ;
#14707 = CONTEXT_DEPENDENT_SHAPE_REPRESENTATION ( #15691, #11021 ) ;
#14708 = CARTESIAN_POINT ( 'NONE',  ( 31.49419854219519976, 9.774809681453278998, 23.00000000000000000 ) ) ;
#14709 = EDGE_CURVE ( 'NONE', #3945, #7334, #17604, .T. ) ;
#14710 = EDGE_CURVE ( 'NONE', #12704, #252, #957, .T. ) ;
#14711 =( BOUNDED_CURVE ( )  B_SPLINE_CURVE ( 2, ( #13821, #22347, #1204 ),
 .UNSPECIFIED., .F., .F. ) 
 B_SPLINE_CURVE_WITH_KNOTS ( ( 3, 3 ),
 ( 0.000000000000000000, 0.2336872276155859962 ),
 .UNSPECIFIED. ) 
 CURVE ( )  GEOMETRIC_REPRESENTATION_ITEM ( )  RATIONAL_B_SPLINE_CURVE ( ( 1.000000000000000000, 1.154700538379259900, 1.000000000000000000 ) ) 
 REPRESENTATION_ITEM ( '' )  );
#14712 =( LENGTH_UNIT ( ) NAMED_UNIT ( * ) SI_UNIT ( .MILLI., .METRE. ) );
#14713 = DIRECTION ( 'NONE',  ( 0.2306359803922053142, 0.9730401042858028982, 0.000000000000000000 ) ) ;
#14714 = PERSON_AND_ORGANIZATION ( #11966, #8758 ) ;
#14715 = EDGE_LOOP ( 'NONE', ( #18196, #11912, #10418, #286 ) ) ;
#14716 = CIRCLE ( 'NONE', #20409, 5.000000000000000888 ) ;
#14717 = PLANE ( 'NONE',  #19036 ) ;
#14718 = ORIENTED_EDGE ( 'NONE', *, *, #20158, .F. ) ;
#14719 = CARTESIAN_POINT ( 'NONE',  ( -17.50000000000000000, -20.00000000000000000, -2.500000000000000000 ) ) ;
#14721 = AXIS2_PLACEMENT_3D ( 'NONE', #6702, #20707, #4907 ) ;
#14720 = FACE_OUTER_BOUND ( 'NONE', #11619, .T. ) ;
#14722 = LINE ( 'NONE', #13647, #13780 ) ;
#14723 = ORIENTED_EDGE ( 'NONE', *, *, #6152, .T. ) ;
#14724 = ORIENTED_EDGE ( 'NONE', *, *, #12136, .F. ) ;
#14725 = LINE ( 'NONE', #20662, #356 ) ;
#14726 = ORIENTED_EDGE ( 'NONE', *, *, #18932, .F. ) ;
#14727 = PERSON_AND_ORGANIZATION ( #11966, #8758 ) ;
#14728 = ADVANCED_FACE ( 'NONE', ( #17363 ), #22568, .T. ) ;
#14729 = EDGE_LOOP ( 'NONE', ( #14618, #2980, #5005, #18280 ) ) ;
#14730 = VERTEX_POINT ( 'NONE', #11796 ) ;
#14731 = DIRECTION ( 'NONE',  ( 1.138590270679731958E-14, 2.220446049251235259E-15, 1.000000000000000000 ) ) ;
#14732 = DIRECTION ( 'NONE',  ( -0.9999862922474492821, -0.005235963827121953122, 1.239088197126291310E-16 ) ) ;
#14733 = APPLICATION_PROTOCOL_DEFINITION ( 'international standard', 'config_control_design', 1994, #7768 ) ;
#14734 = APPLICATION_CONTEXT ( 'configuration controlled 3d designs of mechanical parts and assemblies' ) ;
#14735 = CARTESIAN_POINT ( 'NONE',  ( 36.76586756491558816, 21.07724224331880336, -14.00000000000048672 ) ) ;
#14736 = APPROVAL ( #18609, 'UNSPECIFIED' ) ;
#14737 = CC_DESIGN_DATE_AND_TIME_ASSIGNMENT ( #18019, #11351, ( #6898 ) ) ;
#14738 = DIRECTION ( 'NONE',  ( -0.2306359803922033991, -0.9730401042858034533, 0.000000000000000000 ) ) ;
#14739 = EDGE_CURVE ( 'NONE', #16163, #2081, #12059, .T. ) ;
#14740 = EDGE_CURVE ( 'NONE', #577, #746, #12144, .T. ) ;
#14741 = EDGE_CURVE ( 'NONE', #5544, #12945, #268, .T. ) ;
#14742 = CLOSED_SHELL ( 'NONE', ( #9649, #12425, #4644, #3094, #22562, #9116 ) ) ;
#14743 = VECTOR ( 'NONE', #18387, 1000.000000000000114 ) ;
#14744 = ORIENTED_EDGE ( 'NONE', *, *, #7913, .T. ) ;
#14745 = ADVANCED_BREP_SHAPE_REPRESENTATION ( '', ( #9171, #12739 ), #21598 ) ;
#14746 = LINE ( 'NONE', #11086, #21921 ) ;
#14747 = CALENDAR_DATE ( 2026, 31, 10 ) ;
#14748 = ORIENTED_EDGE ( 'NONE', *, *, #19093, .F. ) ;
#14749 = CARTESIAN_POINT ( 'NONE',  ( 114.2412296582679971, -24.79605227811670076, -2.999999999999940048 ) ) ;
#14750 = DIRECTION ( 'NONE',  ( -1.466984912809907930E-16, -2.805478249466190329E-20, -1.000000000000000000 ) ) ;
#14751 = DIRECTION ( 'NONE',  ( 0.7070970883417638797, 0.003702385528197197663, -0.7071067811865479058 ) ) ;
#14752 = DIRECTION ( 'NONE',  ( 2.982858504577314686E-17, -2.441916418604790135E-15, -1.000000000000000000 ) ) ;
#14753 = CARTESIAN_POINT ( 'NONE',  ( -20.00000002229178619, 25.70208919256900160, 8.500000000004453327 ) ) ;
#14754 = EDGE_LOOP ( 'NONE', ( #13653, #7872, #16416, #21069 ) ) ;
#14755 = CYLINDRICAL_SURFACE ( 'NONE', #18315, 7.000000000000000000 ) ;
#14756 = EDGE_CURVE ( 'NONE', #2526, #7180, #1785, .T. ) ;
#14757 = EDGE_LOOP ( 'NONE', ( #16668, #17557, #14121, #19321, #4272 ) ) ;
#14758 = VERTEX_POINT ( 'NONE', #8576 ) ;
#14759 = DIRECTION ( 'NONE',  ( 0.000000000000000000, -1.000000000000000000, 0.000000000000000000 ) ) ;
#14760 = DIRECTION ( 'NONE',  ( 0.9730401042858035643, -0.2306359803922028717, -5.959266323858674978E-17 ) ) ;
#14761 = VERTEX_POINT ( 'NONE', #21037 ) ;
#14762 = DIRECTION ( 'NONE',  ( 0.2306359803922080620, 0.9730401042858023430, 5.073893018238513068E-14 ) ) ;
#14763 = EDGE_LOOP ( 'NONE', ( #7932, #13408, #16916, #12757, #12827, #16839 ) ) ;
#14764 = DIRECTION ( 'NONE',  ( -0.005235963827101446089, 0.9999862922474493931, 5.936218956632777928E-19 ) ) ;
#14765 = LOCAL_TIME ( 14, 11, 27.00000000000000000, #15588 ) ;
#14766 = SECURITY_CLASSIFICATION_LEVEL ( 'unclassified' ) ;
#14767 = VECTOR ( 'NONE', #20344, 999.9999999999998863 ) ;
#14768 = DIRECTION ( 'NONE',  ( 3.959184095919419975E-16, -4.969292347292200534E-15, -1.000000000000000000 ) ) ;
#14769 = EDGE_CURVE ( 'NONE', #104, #9613, #2933, .T. ) ;
#14770 = EDGE_CURVE ( 'NONE', #20578, #10522, #15566, .T. ) ;
#14771 =( LENGTH_UNIT ( ) NAMED_UNIT ( * ) SI_UNIT ( .MILLI., .METRE. ) );
#14772 = CARTESIAN_POINT ( 'NONE',  ( 66.60056952104010008, 2.425487965306460048, 1.173314102775059961E-14 ) ) ;
#14773 = DIRECTION ( 'NONE',  ( -6.662112528310618598E-09, 1.000000000000000000, -2.220444537147720967E-15 ) ) ;
#14774 = CALENDAR_DATE ( 2026, 31, 10 ) ;
#14775 = CARTESIAN_POINT ( 'NONE',  ( -17.50000000397270128, 22.95208920922877738, 8.000000000004432010 ) ) ;
#14776 = CARTESIAN_POINT ( 'NONE',  ( -58.58222095029707077, 7.653029331589754847, -2.499999999999991118 ) ) ;
#14777 = CARTESIAN_POINT ( 'NONE',  ( 89.62416413250200264, 10.32848256004250054, -13.00000000000030020 ) ) ;
#14778 = DIRECTION ( 'NONE',  ( -0.9730401042858036753, 0.2306359803922028995, -2.804983810440358801E-16 ) ) ;
#14779 = AXIS2_PLACEMENT_3D ( 'NONE', #22029, #22149, #6609 ) ;
#14780 = LINE ( 'NONE', #5756, #21000 ) ;
#14781 = CIRCLE ( 'NONE', #19350, 5.000000000000004441 ) ;
#14782 = CARTESIAN_POINT ( 'NONE',  ( 36.07092311366584880, 11.78608357701223852, 8.759424124907040365 ) ) ;
#14783 = ORIENTED_EDGE ( 'NONE', *, *, #20154, .T. ) ;
#14784 = ADVANCED_FACE ( 'NONE', ( #11929 ), #23029, .T. ) ;
#14785 = ORIENTED_EDGE ( 'NONE', *, *, #20418, .T. ) ;
#14786 = CARTESIAN_POINT ( 'NONE',  ( 33.27705887009690144, -3.036156860537079893, 9.625000000000159872 ) ) ;
#14787 = DIRECTION ( 'NONE',  ( -3.332943903795901177E-07, 0.000000000000000000, 0.9999999999999444888 ) ) ;
#14788 = ORIENTED_EDGE ( 'NONE', *, *, #8240, .T. ) ;
#14789 = LINE ( 'NONE', #3864, #19459 ) ;
#14790 = VERTEX_POINT ( 'NONE', #17468 ) ;
#14791 = CARTESIAN_POINT ( 'NONE',  ( 58.73439644601031517, 17.65016624305016890, -10.99076000000046172 ) ) ;
#14792 = ADVANCED_FACE ( 'NONE', ( #19368 ), #13670, .T. ) ;
#14793 = CALENDAR_DATE ( 2026, 31, 10 ) ;
#14794 = DIRECTION ( 'NONE',  ( 0.9730401042858036753, -0.2306359803922031493, 2.804983810440361760E-16 ) ) ;
#14795 = EDGE_CURVE ( 'NONE', #15535, #21873, #8215, .T. ) ;
#14796 = PRODUCT_DEFINITION_SHAPE ( 'NONE', 'NONE',  #23476 ) ;
#14797 = CC_DESIGN_APPROVAL ( #4067, ( #1591 ) ) ;
#14798 = APPROVAL_STATUS ( 'not_yet_approved' ) ;
#14799 = CARTESIAN_POINT ( 'NONE',  ( 41.61257896558653613, 13.48683030092277235, 3.881831259975344606E-14 ) ) ;
#14800 = CIRCLE ( 'NONE', #18563, 3.000000000000001332 ) ;
#14801 = ORIENTED_EDGE ( 'NONE', *, *, #10326, .T. ) ;
#14802 = LINE ( 'NONE', #183, #18744 ) ;
#14803 = ORIENTED_EDGE ( 'NONE', *, *, #6057, .F. ) ;
#14804 = DIRECTION ( 'NONE',  ( -0.005235963827117092427, 0.9999862922474493931, 2.636227439667000721E-16 ) ) ;
#14805 = FACE_OUTER_BOUND ( 'NONE', #15804, .T. ) ;
#14806 = ORIENTED_EDGE ( 'NONE', *, *, #5050, .F. ) ;
#14807 = VECTOR ( 'NONE', #8706, 1000.000000000000227 ) ;
#14808 = DIRECTION ( 'NONE',  ( 0.000000000000000000, 0.000000000000000000, -1.000000000000000000 ) ) ;
#14809 = CARTESIAN_POINT ( 'NONE',  ( 114.9405074087380001, 12.84085624101770051, 2.283500000000028951 ) ) ;
#14810 = LINE ( 'NONE', #7458, #8015 ) ;
#14811 = ORIENTED_EDGE ( 'NONE', *, *, #4041, .T. ) ;
#14812 = PRODUCT_DEFINITION_FORMATION_WITH_SPECIFIED_SOURCE ( 'ANY', '', #19329, .NOT_KNOWN. ) ;
#14813 = LINE ( 'NONE', #16948, #18687 ) ;
#14814 = LOCAL_TIME ( 14, 11, 27.00000000000000000, #11480 ) ;
#14815 = VERTEX_POINT ( 'NONE', #10369 ) ;
#14816 = CC_DESIGN_PERSON_AND_ORGANIZATION_ASSIGNMENT ( #11357, #13237, ( #7139 ) ) ;
#14817 = CALENDAR_DATE ( 2026, 31, 10 ) ;
#14818 = LINE ( 'NONE', #11179, #10017 ) ;
#14819 = ORIENTED_EDGE ( 'NONE', *, *, #20444, .F. ) ;
#14820 = VERTEX_POINT ( 'NONE', #8330 ) ;
#14821 = LINE ( 'NONE', #439, #9990 ) ;
#14822 = PERSON_AND_ORGANIZATION ( #11966, #8758 ) ;
#14823 = CIRCLE ( 'NONE', #22764, 2.499999999999999112 ) ;
#14824 = DIRECTION ( 'NONE',  ( -0.9997651245102160411, -0.02167246670483410909, 0.000000000000000000 ) ) ;
#14825 = DIRECTION ( 'NONE',  ( -0.9730401042858024541, 0.2306359803922080898, 5.959266323858942451E-17 ) ) ;
#14826 = LOCAL_TIME ( 14, 11, 27.00000000000000000, #16478 ) ;
#14827 = CC_DESIGN_APPROVAL ( #2186, ( #12933 ) ) ;
#14828 = DIRECTION ( 'NONE',  ( 0.3034590813640733464, -0.9528444710117558447, 2.502071977558823078E-16 ) ) ;
#14829 = EDGE_CURVE ( 'NONE', #4562, #11214, #13803, .T. ) ;
#14830 = DATE_AND_TIME ( #16720, #9881 ) ;
#14831 = ORIENTED_EDGE ( 'NONE', *, *, #19681, .T. ) ;
#14832 = CC_DESIGN_APPROVAL ( #21957, ( #1558 ) ) ;
#14833 = DIRECTION ( 'NONE',  ( 0.000000000000000000, -1.000000000000000000, 2.081668171172168119E-15 ) ) ;
#14834 = ORIENTED_EDGE ( 'NONE', *, *, #13132, .T. ) ;
#14835 = CARTESIAN_POINT ( 'NONE',  ( 28.88391017762856450, 3.143668749127940920, -13.00000000000000000 ) ) ;
#14836 = DIRECTION ( 'NONE',  ( 1.000000000000000000, 9.249025156865542385E-11, -2.269596547736322531E-13 ) ) ;
#14837 = DIRECTION ( 'NONE',  ( 0.000000000000000000, -1.000000000000000000, 2.081668171172169697E-15 ) ) ;
#14838 = VERTEX_POINT ( 'NONE', #2979 ) ;
#14839 = ORIENTED_EDGE ( 'NONE', *, *, #5160, .F. ) ;
#14840 = CARTESIAN_POINT ( 'NONE',  ( -20.00000000397420052, 22.95208919256889857, -6.499999999995379696 ) ) ;
#14841 = EDGE_LOOP ( 'NONE', ( #8724, #4984, #22554, #14497 ) ) ;
#14842 = EDGE_CURVE ( 'NONE', #14586, #20287, #2633, .T. ) ;
#14843 = APPROVAL_ROLE ( '' ) ;
#14844 = CC_DESIGN_APPROVAL ( #15767, ( #19398 ) ) ;
#14845 = ORIENTED_EDGE ( 'NONE', *, *, #21771, .F. ) ;
#14846 = EDGE_LOOP ( 'NONE', ( #5662, #18728, #18170, #12293 ) ) ;
#14847 = CARTESIAN_POINT ( 'NONE',  ( 35.59419854219520118, 9.774809681453278998, -23.00000000000000000 ) ) ;
#14848 = DIRECTION ( 'NONE',  ( 1.000000000000000000, 0.000000000000000000, 0.000000000000000000 ) ) ;
#14849 = CALENDAR_DATE ( 2026, 31, 10 ) ;
#14850 = AXIS2_PLACEMENT_3D ( 'NONE', #20767, #4498, #10337 ) ;
#14851 = LINE ( 'NONE', #11436, #9355 ) ;
#14852 = VECTOR ( 'NONE', #12284, 999.9999999999998863 ) ;
#14853 = DIRECTION ( 'NONE',  ( 1.159535895544890222E-14, 2.167612681253619929E-15, 1.000000000000000000 ) ) ;
#14854 = LOCAL_TIME ( 14, 11, 27.00000000000000000, #7797 ) ;
#14855 = EDGE_LOOP ( 'NONE', ( #4964, #13640, #3699, #11207, #22691, #13520 ) ) ;
#14856 = CARTESIAN_POINT ( 'NONE',  ( 34.89491389100810181, 23.30074776265909975, -13.00000000000049916 ) ) ;
#14857 = EDGE_CURVE ( 'NONE', #13198, #22018, #13908, .T. ) ;
#14858 = COORDINATED_UNIVERSAL_TIME_OFFSET ( 0, 0, .AHEAD. ) ;
#14859 = SECURITY_CLASSIFICATION ( '', '', #11325 ) ;
#14860 = ORIENTED_EDGE ( 'NONE', *, *, #15824, .T. ) ;
#14861 = CARTESIAN_POINT ( 'NONE',  ( -25.00000000000000000, -20.00000000000000000, 0.000000000000000000 ) ) ;
#14862 = AXIS2_PLACEMENT_3D ( 'NONE', #15, #23419, #1693 ) ;
#14863 = DIRECTION ( 'NONE',  ( 1.138590270679730064E-14, 2.220446049251240387E-15, 1.000000000000000000 ) ) ;
#14864 = APPROVAL ( #5456, 'UNKNOWN' ) ;
#14865 = CARTESIAN_POINT ( 'NONE',  ( 30.50389457288209982, -2.378844316418859517, -13.00000000000000000 ) ) ;
#14866 = VECTOR ( 'NONE', #17203, 1000.000000000000114 ) ;
#14867 = CC_DESIGN_DATE_AND_TIME_ASSIGNMENT ( #1554, #3936, ( #5761 ) ) ;
#14868 = VECTOR ( 'NONE', #19065, 1000.000000000000114 ) ;
#14869 = CARTESIAN_POINT ( 'NONE',  ( 0.7956971858519210627, 15.29954237522671967, -7.022951190117520595E-15 ) ) ;
#14870 = EDGE_LOOP ( 'NONE', ( #14702, #8582, #4426, #19818, #14916, #5713, #5179, #21641, #19599, #8310, #3283, #15112, #13464, #1998 ) ) ;
#14871 = LOCAL_TIME ( 14, 11, 27.00000000000000000, #12085 ) ;
#14872 = DIRECTION ( 'NONE',  ( 0.9730401042858024541, -0.2306359803922080898, -5.959266323858942451E-17 ) ) ;
#14873 = DESIGN_CONTEXT ( 'detailed design', #21555, 'design' ) ;
#14874 = EDGE_CURVE ( 'NONE', #13130, #7633, #13558, .T. ) ;
#14875 = ADVANCED_FACE ( 'NONE', ( #2869 ), #8687, .T. ) ;
#14876 = AXIS2_PLACEMENT_3D ( 'NONE', #15455, #12151, #12276 ) ;
#14877 = ORIENTED_EDGE ( 'NONE', *, *, #15269, .T. ) ;
#14878 = ORIENTED_EDGE ( 'NONE', *, *, #20871, .T. ) ;
#14879 = FACE_OUTER_BOUND ( 'NONE', #14980, .T. ) ;
#14880 = DIRECTION ( 'NONE',  ( -1.000000000000000000, 0.000000000000000000, 0.000000000000000000 ) ) ;
#14881 = VERTEX_POINT ( 'NONE', #19493 ) ;
#14882 = CARTESIAN_POINT ( 'NONE',  ( 114.2412296582679971, -24.79605227811680379, 3.000000000000000000 ) ) ;
#14883 = CC_DESIGN_APPROVAL ( #12859, ( #8452 ) ) ;
#14884 = CARTESIAN_POINT ( 'NONE',  ( -20.80722593534541076, 19.54644882756858948, -2.500000000000000000 ) ) ;
#14885 = VECTOR ( 'NONE', #23385, 1000.000000000000000 ) ;
#14886 = DIRECTION ( 'NONE',  ( 1.000000000000000000, 0.000000000000000000, 1.480297366166879989E-16 ) ) ;
#14887 = CIRCLE ( 'NONE', #6157, 4.099999999999999645 ) ;
#14888 = VECTOR ( 'NONE', #18136, 999.9999999999998863 ) ;
#14889 = DIRECTION ( 'NONE',  ( -1.000000000000000000, 0.000000000000000000, 0.000000000000000000 ) ) ;
#14890 = AXIS2_PLACEMENT_3D ( 'NONE', #14182, #3362, #8367 ) ;
#14891 = CARTESIAN_POINT ( 'NONE',  ( -26.75617730459320143, 6.359992804688680224, 9.266501092714649290E-14 ) ) ;
#14892 = EDGE_CURVE ( 'NONE', #18732, #12554, #4831, .T. ) ;
#14893 = PERSON_AND_ORGANIZATION ( #11966, #8758 ) ;
#14894 = LINE ( 'NONE', #2437, #2049 ) ;
#14895 = AXIS2_PLACEMENT_3D ( 'NONE', #19355, #23129, #6894 ) ;
#14896 = DIRECTION ( 'NONE',  ( -0.2306359803922028995, -0.9730401042858036753, 1.343075398093749487E-16 ) ) ;
#14897 = CIRCLE ( 'NONE', #17944, 2.500000000000000000 ) ;
#14898 = APPROVAL ( #17208, 'UNSPECIFIED' ) ;
#14899 = LINE ( 'NONE', #739, #11654 ) ;
#14900 = CC_DESIGN_APPROVAL ( #21986, ( #15292 ) ) ;
#14901 = DIRECTION ( 'NONE',  ( -2.979612008695687415E-09, 0.4472135954999595375, -0.8944271909999150783 ) ) ;
#14902 = CC_DESIGN_DATE_AND_TIME_ASSIGNMENT ( #16392, #8932, ( #14054 ) ) ;
#14903 = DIRECTION ( 'NONE',  ( 0.000000000000000000, 1.020425574104004122E-16, 1.000000000000000000 ) ) ;
#14904 = CIRCLE ( 'NONE', #6180, 2.749999999999999112 ) ;
#14905 = DIRECTION ( 'NONE',  ( 0.2306359803922028717, 0.9730401042858035643, -7.445392196378163890E-17 ) ) ;
#14906 = ADVANCED_FACE ( 'NONE', ( #19718 ), #19629, .T. ) ;
#14907 = VECTOR ( 'NONE', #3608, 1000.000000000000114 ) ;
#14909 = ORIENTED_EDGE ( 'NONE', *, *, #22866, .F. ) ;
#14908 = EDGE_CURVE ( 'NONE', #2588, #1063, #5467, .T. ) ;
#14910 = AXIS2_PLACEMENT_3D ( 'NONE', #18102, #3721, #5736 ) ;
#14911 = EDGE_LOOP ( 'NONE', ( #3894, #20064, #9703, #6922, #13771, #4238 ) ) ;
#14912 = DIRECTION ( 'NONE',  ( 0.000000000000000000, 0.000000000000000000, 1.000000000000000000 ) ) ;
#14913 = PLANE ( 'NONE',  #18615 ) ;
#14914 = EDGE_LOOP ( 'NONE', ( #214, #18768, #20947, #4377 ) ) ;
#14915 = CARTESIAN_POINT ( 'NONE',  ( 34.14207834813670672, 22.29249582057180135, -11.00000000000049916 ) ) ;
#14916 = ORIENTED_EDGE ( 'NONE', *, *, #21539, .F. ) ;
#14917 = DIRECTION ( 'NONE',  ( 0.7806762821593219437, -0.6249356306643899517, -1.755540157688528780E-13 ) ) ;
#14918 = PERSON_AND_ORGANIZATION_ROLE ( 'creator' ) ;
#14919 = CARTESIAN_POINT ( 'NONE',  ( 37.42446263180998756, 10.74467201676272943, -8.896276805998382997 ) ) ;
#14920 = CC_DESIGN_APPROVAL ( #6762, ( #17596 ) ) ;
#14921 = VECTOR ( 'NONE', #13385, 999.9999999999998863 ) ;
#14922 = APPROVAL_ROLE ( '' ) ;
#14923 = SHAPE_REPRESENTATION_RELATIONSHIP ( 'NONE' , 'NONE' ,  #5348, #13615 ) ;
#14924 =( REPRESENTATION_RELATIONSHIP ('NONE','NONE', #18121, #10862 ) REPRESENTATION_RELATIONSHIP_WITH_TRANSFORMATION ( #20412 )SHAPE_REPRESENTATION_RELATIONSHIP( ) );
#14925 = AXIS2_PLACEMENT_3D ( 'NONE', #1835, #2074, #12546 ) ;
#14926 = DIRECTION ( 'NONE',  ( -0.9730401042858035643, 0.2306359803922031215, -2.804983810440351899E-16 ) ) ;
#14927 = ORIENTED_EDGE ( 'NONE', *, *, #19277, .F. ) ;
#14928 = ADVANCED_FACE ( 'NONE', ( #21490 ), #14370, .T. ) ;
#14929 = AXIS2_PLACEMENT_3D ( 'NONE', #5078, #4830, #16107 ) ;
#14930 = CARTESIAN_POINT ( 'NONE',  ( 118.5079952955230027, -6.794810348829359192, -15.50000000000000000 ) ) ;
#14931 = ORIENTED_EDGE ( 'NONE', *, *, #11189, .F. ) ;
#14932 = DIRECTION ( 'NONE',  ( 2.982858504577319616E-17, -2.441916418604790135E-15, -1.000000000000000000 ) ) ;
#14933 = DIRECTION ( 'NONE',  ( 0.000000000000000000, 0.000000000000000000, 1.000000000000000000 ) ) ;
#14934 = ORIENTED_EDGE ( 'NONE', *, *, #4247, .T. ) ;
#14935 = CARTESIAN_POINT ( 'NONE',  ( 35.34171762861030430, 30.38879166913060104, 15.99999999999969802 ) ) ;
#14936 = CARTESIAN_POINT ( 'NONE',  ( -26.72214353971689960, -0.1399180949199889945, 2.500999999999910184 ) ) ;
#14937 = LINE ( 'NONE', #10810, #13318 ) ;
#14938 = ORIENTED_EDGE ( 'NONE', *, *, #3909, .F. ) ;
#14939 = ADVANCED_FACE ( 'NONE', ( #7032 ), #12439, .F. ) ;
#14940 = AXIS2_PLACEMENT_3D ( 'NONE', #3162, #17659, #8625 ) ;
#14941 = ADVANCED_FACE ( 'NONE', ( #3444, #3331 ), #14252, .T. ) ;
#14942 = DIRECTION ( 'NONE',  ( 1.000000000000000000, 0.000000000000000000, 1.480297366166879989E-16 ) ) ;
#14943 = CIRCLE ( 'NONE', #4704, 2.500000000000000444 ) ;
#14944 = VERTEX_POINT ( 'NONE', #7144 ) ;
#14945 = COORDINATED_UNIVERSAL_TIME_OFFSET ( 0, 0, .AHEAD. ) ;
#14946 = CARTESIAN_POINT ( 'NONE',  ( 5.000000000000000000, -27.34999999999999787, -6.250000000000000000 ) ) ;
#14947 = VERTEX_POINT ( 'NONE', #21386 ) ;
#14948 = ORIENTED_EDGE ( 'NONE', *, *, #7667, .T. ) ;
#14949 = DIRECTION ( 'NONE',  ( -0.9997648975362221080, -0.02168293463503390486, 0.000000000000000000 ) ) ;
#14950 = DATE_AND_TIME ( #9487, #20949 ) ;
#14951 = CALENDAR_DATE ( 2026, 31, 10 ) ;
#14952 = CARTESIAN_POINT ( 'NONE',  ( -26.75617730459320143, 6.359992804688680224, 2.500000000000090150 ) ) ;
#14953 = DIRECTION ( 'NONE',  ( 0.000000000000000000, 0.000000000000000000, -1.000000000000000000 ) ) ;
#14954 = CC_DESIGN_PERSON_AND_ORGANIZATION_ASSIGNMENT ( #4306, #12849, ( #4599 ) ) ;
#14955 = APPROVAL_ROLE ( '' ) ;
#14956 = ADVANCED_FACE ( 'NONE', ( #10716 ), #8246, .F. ) ;
#14957 = ORIENTED_EDGE ( 'NONE', *, *, #12740, .T. ) ;
#14958 = DIRECTION ( 'NONE',  ( 0.9822610636820822139, -0.1875185398144529336, 5.059610138265687687E-16 ) ) ;
#14959 = ORIENTED_EDGE ( 'NONE', *, *, #16481, .F. ) ;
#14960 = LINE ( 'NONE', #20422, #19256 ) ;
#14961 = CARTESIAN_POINT ( 'NONE',  ( 37.01481097301077483, 22.79827665208033238, 15.00000000000000178 ) ) ;
#14962 = DIRECTION ( 'NONE',  ( 0.000000000000000000, 0.000000000000000000, 1.000000000000000000 ) ) ;
#14963 = ORIENTED_EDGE ( 'NONE', *, *, #10909, .T. ) ;
#14964 = ORIENTED_EDGE ( 'NONE', *, *, #11862, .F. ) ;
#14965 = FACE_OUTER_BOUND ( 'NONE', #21819, .T. ) ;
#14966 = ORIENTED_EDGE ( 'NONE', *, *, #22532, .T. ) ;
#14967 = SHAPE_DEFINITION_REPRESENTATION ( #3214, #21569 ) ;
#14968 = ORIENTED_EDGE ( 'NONE', *, *, #4675, .T. ) ;
#14969 = ORIENTED_EDGE ( 'NONE', *, *, #12277, .F. ) ;
#14970 = PLANE ( 'NONE',  #274 ) ;
#14971 = COORDINATED_UNIVERSAL_TIME_OFFSET ( 0, 0, .AHEAD. ) ;
#14972 = CARTESIAN_POINT ( 'NONE',  ( 38.22140682376686982, 9.152092534394578038, 26.50000000000000355 ) ) ;
#14973 = ADVANCED_FACE ( 'NONE', ( #10598 ), #15835, .F. ) ;
#14974 = CARTESIAN_POINT ( 'NONE',  ( 37.01481097301078194, 22.79827665208033594, 11.00000000000000178 ) ) ;
#14975 = DIRECTION ( 'NONE',  ( 1.000000000000000000, 0.000000000000000000, 0.000000000000000000 ) ) ;
#14976 = ORIENTED_EDGE ( 'NONE', *, *, #3528, .F. ) ;
#14977 = CARTESIAN_POINT ( 'NONE',  ( -23.50000000000000000, -20.00000000000000000, -5.000000000000000000 ) ) ;
#14978 = APPROVAL_ROLE ( '' ) ;
#14979 = VECTOR ( 'NONE', #205, 1000.000000000000114 ) ;
#14980 = EDGE_LOOP ( 'NONE', ( #7966, #6835, #2521, #17466, #21333 ) ) ;
#14981 = DIRECTION ( 'NONE',  ( 3.837966487416234409E-32, -1.216195237911450118E-15, -1.000000000000000000 ) ) ;
#14982 = DIRECTION ( 'NONE',  ( 3.108182772708750394E-21, -5.936137584479539905E-19, 1.000000000000000000 ) ) ;
#14983 = ORIENTED_EDGE ( 'NONE', *, *, #23434, .F. ) ;
#14984 = CARTESIAN_POINT ( 'NONE',  ( -25.00842861987479893, -15.87143667223269894, 25.00000000000000000 ) ) ;
#14985 = FACE_OUTER_BOUND ( 'NONE', #20752, .T. ) ;
#14986 = EDGE_LOOP ( 'NONE', ( #6847, #4863, #1051, #6046 ) ) ;
#14987 = DIRECTION ( 'NONE',  ( 1.000000000000000000, -1.176672321210050136E-14, 0.000000000000000000 ) ) ;
#14988 = PERSON_AND_ORGANIZATION_ROLE ( 'design_supplier' ) ;
#14989 = PRODUCT_DEFINITION_SHAPE ( 'NONE', 'NONE',  #23509 ) ;
#14990 = EDGE_LOOP ( 'NONE', ( #420, #8341, #16004, #7517, #17693, #12366 ) ) ;
#14991 = ORIENTED_EDGE ( 'NONE', *, *, #23443, .F. ) ;
#14992 = CYLINDRICAL_SURFACE ( 'NONE', #6962, 2.500000000000000444 ) ;
#14993 = CYLINDRICAL_SURFACE ( 'NONE', #6053, 2.499999999999999112 ) ;
#14994 = ORIENTED_EDGE ( 'NONE', *, *, #16957, .T. ) ;
#14995 = PERSON_AND_ORGANIZATION ( #11966, #8758 ) ;
#14996 = DIRECTION ( 'NONE',  ( -0.2306359803922080343, -0.9730401042858022320, 1.015202274805050187E-13 ) ) ;
#14997 = EDGE_CURVE ( 'NONE', #9786, #23152, #6909, .T. ) ;
#14998 = AXIS2_PLACEMENT_3D ( 'NONE', #16460, #14336, #10676 ) ;
#14999 = CARTESIAN_POINT ( 'NONE',  ( -30.72441677844230057, -6.660963241697680282, -5.500000000000089706 ) ) ;
#15000 = COORDINATED_UNIVERSAL_TIME_OFFSET ( 0, 0, .AHEAD. ) ;
#15001 = DIRECTION ( 'NONE',  ( -0.2306359803922019835, -0.9730401042858037863, 4.857225732735059075E-15 ) ) ;
#15002 = CC_DESIGN_PERSON_AND_ORGANIZATION_ASSIGNMENT ( #16117, #10801, ( #62 ) ) ;
#15003 = CIRCLE ( 'NONE', #23349, 2.500000000000000444 ) ;
#15004 =( NAMED_UNIT ( * ) PLANE_ANGLE_UNIT ( ) SI_UNIT ( $, .RADIAN. ) );
#15005 = CARTESIAN_POINT ( 'NONE',  ( -20.00000000000000000, -20.00000000000000000, 2.500000000000000000 ) ) ;
#15006 = EDGE_CURVE ( 'NONE', #7688, #23458, #19952, .T. ) ;
#15007 = EDGE_CURVE ( 'NONE', #6022, #21478, #5589, .T. ) ;
#15008 = DIRECTION ( 'NONE',  ( 6.123230199561459225E-17, 4.868008300101910084E-15, 1.000000000000000000 ) ) ;
#15009 = COORDINATED_UNIVERSAL_TIME_OFFSET ( 0, 0, .AHEAD. ) ;
#15010 = CARTESIAN_POINT ( 'NONE',  ( -19.44579266323601985, -2.601514938066513682, 5.000000000000006217 ) ) ;
#15011 = CARTESIAN_POINT ( 'NONE',  ( 34.15720538308221421, 9.344634530308482567, -27.44000000000048445 ) ) ;
#15012 = CARTESIAN_POINT ( 'NONE',  ( 35.09747506357100377, 11.43410645592859964, 27.68999999999999773 ) ) ;
#15013 = CARTESIAN_POINT ( 'NONE',  ( -20.00000002146277467, 25.57708919256889857, -8.249999999995553779 ) ) ;
#15014 = DIRECTION ( 'NONE',  ( 0.9730401042858035643, -0.2306359803922028717, -5.432877459303547053E-17 ) ) ;
#15015 = LINE ( 'NONE', #20830, #14868 ) ;
#15016 = ORIENTED_EDGE ( 'NONE', *, *, #23206, .F. ) ;
#15017 = ORIENTED_EDGE ( 'NONE', *, *, #4179, .T. ) ;
#15018 = CARTESIAN_POINT ( 'NONE',  ( 120.3930287342899987, 3.035456073538489896, 13.00000000000000000 ) ) ;
#15019 = DIRECTION ( 'NONE',  ( -0.9730401042858020100, 0.2306359803922092278, -1.869849304631841307E-15 ) ) ;
#15020 = ORIENTED_EDGE ( 'NONE', *, *, #17387, .T. ) ;
#15021 = DIRECTION ( 'NONE',  ( 0.000000000000000000, 1.000000000000000000, 0.000000000000000000 ) ) ;
#15022 = EDGE_CURVE ( 'NONE', #17438, #10377, #18171, .T. ) ;
#15023 = ORIENTED_EDGE ( 'NONE', *, *, #19416, .F. ) ;
#15024 = DIRECTION ( 'NONE',  ( 0.9730401042858024541, -0.2306359803922080898, -5.959266323858942451E-17 ) ) ;
#15025 = PERSON_AND_ORGANIZATION ( #11966, #8758 ) ;
#15026 = LINE ( 'NONE', #3991, #22628 ) ;
#15027 = CC_DESIGN_PERSON_AND_ORGANIZATION_ASSIGNMENT ( #9712, #18378, ( #11806 ) ) ;
#15028 = CIRCLE ( 'NONE', #2524, 2.749999999999999112 ) ;
#15029 = APPROVAL ( #19108, 'UNSPECIFIED' ) ;
#15030 = CALENDAR_DATE ( 2026, 31, 10 ) ;
#15031 = CIRCLE ( 'NONE', #2901, 2.500000000000000444 ) ;
#15032 = LINE ( 'NONE', #4468, #22661 ) ;
#15033 = EDGE_CURVE ( 'NONE', #17965, #4802, #4464, .T. ) ;
#15034 = ADVANCED_FACE ( 'NONE', ( #16382 ), #21504, .T. ) ;
#15035 = ORIENTED_EDGE ( 'NONE', *, *, #14403, .T. ) ;
#15036 = CC_DESIGN_PERSON_AND_ORGANIZATION_ASSIGNMENT ( #1433, #8815, ( #21422 ) ) ;
#15037 = DIRECTION ( 'NONE',  ( -0.9730401042858022320, 0.2306359803922080343, 5.959266323858941219E-17 ) ) ;
#15038 = EDGE_CURVE ( 'NONE', #7448, #14326, #18488, .T. ) ;
#15039 = ORIENTED_EDGE ( 'NONE', *, *, #4032, .F. ) ;
#15040 = LINE ( 'NONE', #22272, #12436 ) ;
#15041 = ADVANCED_BREP_SHAPE_REPRESENTATION ( '', ( #9625, #12739 ), #22192 ) ;
#15042 = DIRECTION ( 'NONE',  ( -0.2306359803922053697, -0.9730401042858028982, 0.000000000000000000 ) ) ;
#15043 = VERTEX_POINT ( 'NONE', #17716 ) ;
#15044 = DIRECTION ( 'NONE',  ( 0.000000000000000000, -2.899485473084796609E-46, -1.000000000000000000 ) ) ;
#15045 = CARTESIAN_POINT ( 'NONE',  ( -14.00000000397430000, 22.95208919312840123, -6.749999999996930455 ) ) ;
#15046 = VERTEX_POINT ( 'NONE', #213 ) ;
#15047 =( REPRESENTATION_RELATIONSHIP ('NONE','NONE', #19303, #12037 ) REPRESENTATION_RELATIONSHIP_WITH_TRANSFORMATION ( #7813 )SHAPE_REPRESENTATION_RELATIONSHIP( ) );
#15048 = VECTOR ( 'NONE', #11745, 1000.000000000000000 ) ;
#15049 = PERSON_AND_ORGANIZATION ( #9930, #23204 ) ;
#15050 = DIRECTION ( 'NONE',  ( -2.982858504577314686E-17, 2.441916418604790135E-15, 1.000000000000000000 ) ) ;
#15051 = CIRCLE ( 'NONE', #22617, 2.749999999999999112 ) ;
#15052 = ORIENTED_EDGE ( 'NONE', *, *, #9574, .T. ) ;
#15053 = PERSON_AND_ORGANIZATION ( #11966, #8758 ) ;
#15054 = DIRECTION ( 'NONE',  ( -0.9730401042858024541, 0.2306359803922080898, 5.959266323858942451E-17 ) ) ;
#15055 = EDGE_CURVE ( 'NONE', #23191, #7455, #12939, .T. ) ;
#15056 = VERTEX_POINT ( 'NONE', #22304 ) ;
#15057 = ORIENTED_EDGE ( 'NONE', *, *, #21538, .T. ) ;
#15058 = CARTESIAN_POINT ( 'NONE',  ( 40.45939906362420402, 8.621629779492399948, -1.858156152378089715E-13 ) ) ;
#15059 = PERSON_AND_ORGANIZATION ( #11966, #8758 ) ;
#15060 = SHAPE_REPRESENTATION ( '1602p_c_11', ( #12739 ), #6306 ) ;
#15061 = CIRCLE ( 'NONE', #5196, 2.600000000000000089 ) ;
#15062 = DIRECTION ( 'NONE',  ( 6.123230174520370177E-17, 4.962644601432260272E-15, 1.000000000000000000 ) ) ;
#15063 = EDGE_CURVE ( 'NONE', #18682, #9101, #17353, .T. ) ;
#15064 = EDGE_CURVE ( 'NONE', #10522, #22018, #4593, .T. ) ;
#15065 = AXIS2_PLACEMENT_3D ( 'NONE', #1065, #6426, #20910 ) ;
#15066 = CARTESIAN_POINT ( 'NONE',  ( 0.000000000000000000, 0.000000000000000000, 0.000000000000000000 ) ) ;
#15067 = CARTESIAN_POINT ( 'NONE',  ( -17.50034580627744063, 23.00627559326238369, 2.499999999999900524 ) ) ;
#15068 = EDGE_LOOP ( 'NONE', ( #10202, #9364, #5127, #4996 ) ) ;
#15069 = CALENDAR_DATE ( 2026, 31, 10 ) ;
#15070 = EDGE_LOOP ( 'NONE', ( #7846, #7746, #20375, #16136 ) ) ;
#15071 = AXIS2_PLACEMENT_3D ( 'NONE', #11816, #15470, #13347 ) ;
#15072 = DIRECTION ( 'NONE',  ( 0.2306359803922080898, 0.9730401042858024541, -2.572202231434325988E-16 ) ) ;
#15073 = VERTEX_POINT ( 'NONE', #16605 ) ;
#15074 = CARTESIAN_POINT ( 'NONE',  ( -14.00000000144740042, -4.350228928435730502, 6.750000000004459544 ) ) ;
#15075 = DIRECTION ( 'NONE',  ( 0.005235963827108352890, -0.9999862922474493931, -2.671135040551771006E-18 ) ) ;
#15076 = FACE_BOUND ( 'NONE', #16351, .T. ) ;
#15077 = CIRCLE ( 'NONE', #12432, 4.750000000000000000 ) ;
#15078 = ORIENTED_EDGE ( 'NONE', *, *, #5330, .T. ) ;
#15079 = ORIENTED_EDGE ( 'NONE', *, *, #19251, .F. ) ;
#15080 = CARTESIAN_POINT ( 'NONE',  ( -1.115787625658725135, 15.90677035165398046, 4.486964506765413337E-17 ) ) ;
#15081 = ORIENTED_EDGE ( 'NONE', *, *, #1670, .T. ) ;
#15082 = PERSON_AND_ORGANIZATION ( #11966, #8758 ) ;
#15083 = AXIS2_PLACEMENT_3D ( 'NONE', #1006, #6982, #15629 ) ;
#15084 = ORIENTED_EDGE ( 'NONE', *, *, #2845, .F. ) ;
#15085 = ORIENTED_EDGE ( 'NONE', *, *, #13641, .T. ) ;
#15086 = DIRECTION ( 'NONE',  ( -0.7071067811865475727, 1.387778780781445281E-15, 0.7071067811865475727 ) ) ;
#15087 = AXIS2_PLACEMENT_3D ( 'NONE', #3620, #10777, #1715 ) ;
#15088 = PERSON_AND_ORGANIZATION_ROLE ( 'creator' ) ;
#15089 = DIRECTION ( 'NONE',  ( -0.2306359803922080620, -0.9730401042858023430, 5.397021885244292808E-15 ) ) ;
#15090 = CARTESIAN_POINT ( 'NONE',  ( 37.48968750243700043, 22.68571848161319693, -13.00000000000049916 ) ) ;
#15091 = EDGE_CURVE ( 'NONE', #11874, #21452, #11061, .T. ) ;
#15092 = VECTOR ( 'NONE', #3057, 999.9999999999998863 ) ;
#15093 = ADVANCED_FACE ( 'NONE', ( #2239 ), #14717, .F. ) ;
#15094 =( NAMED_UNIT ( * ) PLANE_ANGLE_UNIT ( ) SI_UNIT ( $, .RADIAN. ) );
#15095 = CIRCLE ( 'NONE', #6389, 2.500000000000000444 ) ;
#15096 = LINE ( 'NONE', #7618, #10955 ) ;
#15097 = DATE_AND_TIME ( #18325, #22030 ) ;
#15098 = AXIS2_PLACEMENT_3D ( 'NONE', #1794, #10505, #16407 ) ;
#15099 = ORIENTED_EDGE ( 'NONE', *, *, #1397, .F. ) ;
#15100 = FACE_OUTER_BOUND ( 'NONE', #7211, .T. ) ;
#15101 = CARTESIAN_POINT ( 'NONE',  ( 34.28138625273830087, 8.929810336689708805, -29.25000000000050093 ) ) ;
#15102 = VERTEX_POINT ( 'NONE', #329 ) ;
#15103 = LINE ( 'NONE', #841, #6336 ) ;
#15104 = DIRECTION ( 'NONE',  ( 1.187319687680494078E-16, 2.805478249478345354E-20, 1.000000000000000000 ) ) ;
#15105 = ORIENTED_EDGE ( 'NONE', *, *, #1114, .F. ) ;
#15106 = DIRECTION ( 'NONE',  ( -0.005235963827117252022, 0.9999862922474493931, 3.469446951953616307E-19 ) ) ;
#15107 = CALENDAR_DATE ( 2026, 31, 10 ) ;
#15108 = ORIENTED_EDGE ( 'NONE', *, *, #8570, .F. ) ;
#15109 = ORIENTED_EDGE ( 'NONE', *, *, #15327, .F. ) ;
#15110 = DIRECTION ( 'NONE',  ( 0.2306359803922077290, 0.9730401042858024541, -1.412237191019971018E-17 ) ) ;
#15111 = CARTESIAN_POINT ( 'NONE',  ( 35.59419854219520118, 9.774809681453278998, -25.00000000000000000 ) ) ;
#15112 = ORIENTED_EDGE ( 'NONE', *, *, #17372, .F. ) ;
#15113 = APPROVAL_ROLE ( '' ) ;
#15114 = CARTESIAN_POINT ( 'NONE',  ( -62.91457587699539289, 8.067188213978639055, 2.213507334852100055E-15 ) ) ;
#15115 = CARTESIAN_POINT ( 'NONE',  ( -19.77176037304764833, 27.94687714311316284, 5.000000000004446221 ) ) ;
#15116 = VECTOR ( 'NONE', #22159, 1000.000000000000000 ) ;
#15117 = CARTESIAN_POINT ( 'NONE',  ( -14.00000000202540029, 1.899127378930379972, 6.750000000004440004 ) ) ;
#15118 = PLANE ( 'NONE',  #21745 ) ;
#15119 = DIRECTION ( 'NONE',  ( 3.211814849206744928E-17, -2.442368445299930211E-15, -1.000000000000000000 ) ) ;
#15120 = APPROVAL_DATE_TIME ( #20120, #2920 ) ;
#15121 = CARTESIAN_POINT ( 'NONE',  ( -19.49999999982360066, -0.1021026942259700004, 2.500000000000000000 ) ) ;
#15122 = FACE_OUTER_BOUND ( 'NONE', #9064, .T. ) ;
#15123 = EDGE_CURVE ( 'NONE', #4764, #9507, #5824, .T. ) ;
#15124 = FACE_BOUND ( 'NONE', #7877, .T. ) ;
#15125 = ADVANCED_FACE ( 'NONE', ( #6045 ), #18533, .T. ) ;
#15126 = DIRECTION ( 'NONE',  ( -0.9730401042858035643, 0.2306359803922028717, -2.804983810440358308E-16 ) ) ;
#15127 = DIRECTION ( 'NONE',  ( -0.9999862922474492821, -0.005235963827121951387, 1.239088197126291310E-16 ) ) ;
#15128 = FACE_OUTER_BOUND ( 'NONE', #16087, .T. ) ;
#15129 = ORIENTED_EDGE ( 'NONE', *, *, #8486, .F. ) ;
#15130 = EDGE_LOOP ( 'NONE', ( #538, #21669, #21675, #20082, #17341, #18545, #18245, #2315 ) ) ;
#15131 = CARTESIAN_POINT ( 'NONE',  ( -1.613230144398002386, 26.81559938783153996, -8.272051826996034682E-16 ) ) ;
#15132 = CARTESIAN_POINT ( 'NONE',  ( -28.52462712253550237, 6.350733138482030249, -0.7325259402521649976 ) ) ;
#15133 = VERTEX_POINT ( 'NONE', #20307 ) ;
#15134 = CIRCLE ( 'NONE', #10245, 2.500000000028980374 ) ;
#15135 = EDGE_CURVE ( 'NONE', #8287, #6032, #690, .T. ) ;
#15136 = DIRECTION ( 'NONE',  ( -0.9730401042858035643, 0.2306359803922028717, 5.958148513035547083E-17 ) ) ;
#15137 = ORIENTED_EDGE ( 'NONE', *, *, #20798, .F. ) ;
#15138 = LINE ( 'NONE', #2322, #10945 ) ;
#15139 = DATE_AND_TIME ( #4354, #17181 ) ;
#15140 = CARTESIAN_POINT ( 'NONE',  ( 35.34171762861030430, 30.38879166913060104, 19.99999999999969802 ) ) ;
#15141 = ITEM_DEFINED_TRANSFORMATION ( 'NONE', 'NONE', #21220,  #12739 ) ;
#15142 = FACE_OUTER_BOUND ( 'NONE', #10351, .T. ) ;
#15143 = DIRECTION ( 'NONE',  ( -0.005235963827110212514, 0.9999862922474493931, 5.936218956700083401E-19 ) ) ;
#15144 = ORIENTED_EDGE ( 'NONE', *, *, #3425, .F. ) ;
#15145 = LOCAL_TIME ( 14, 11, 27.00000000000000000, #22824 ) ;
#15146 = DIRECTION ( 'NONE',  ( -0.9730401042858036753, 0.2306359803922028995, -2.355138688025664352E-16 ) ) ;
#15147 = AXIS2_PLACEMENT_3D ( 'NONE', #9759, #22313, #11664 ) ;
#15148 = ORIENTED_EDGE ( 'NONE', *, *, #7751, .F. ) ;
#15149 = CARTESIAN_POINT ( 'NONE',  ( 36.50043006307940630, 22.92019839501219991, 12.99999999999979927 ) ) ;
#15150 = ADVANCED_FACE ( 'NONE', ( #9381 ), #11549, .T. ) ;
#15151 = DIRECTION ( 'NONE',  ( -0.2306359803922102825, -0.9730401042858017879, 4.163336342344335449E-15 ) ) ;
#15152 = ORIENTED_EDGE ( 'NONE', *, *, #3193, .T. ) ;
#15153 = AXIS2_PLACEMENT_3D ( 'NONE', #7545, #1833, #9087 ) ;
#15154 = DIRECTION ( 'NONE',  ( 2.270069654138870255E-15, 1.000000000000000000, 7.035747901516317327E-77 ) ) ;
#15155 = CYLINDRICAL_SURFACE ( 'NONE', #4972, 2.499999999999997780 ) ;
#15156 = ORIENTED_EDGE ( 'NONE', *, *, #14741, .F. ) ;
#15157 = APPROVAL ( #18983, 'UNKNOWN' ) ;
#15158 = APPROVAL_DATE_TIME ( #22629, #15302 ) ;
#15159 = CC_DESIGN_PERSON_AND_ORGANIZATION_ASSIGNMENT ( #124, #18436, ( #19382 ) ) ;
#15160 = DIRECTION ( 'NONE',  ( 8.911056267098788616E-18, 1.998401444326210262E-15, 1.000000000000000000 ) ) ;
#15161 = ORIENTED_EDGE ( 'NONE', *, *, #9723, .T. ) ;
#15162 = EDGE_CURVE ( 'NONE', #16805, #638, #17501, .T. ) ;
#15163 = ADVANCED_FACE ( 'NONE', ( #22189 ), #9500, .F. ) ;
#15164 = DATE_AND_TIME ( #11529, #22399 ) ;
#15165 = DIRECTION ( 'NONE',  ( -2.269700743865584947E-13, -2.220446049247695246E-15, -1.000000000000000000 ) ) ;
#15166 = ORIENTED_EDGE ( 'NONE', *, *, #21393, .T. ) ;
#15167 = LOCAL_TIME ( 14, 11, 27.00000000000000000, #22068 ) ;
#15168 = EDGE_LOOP ( 'NONE', ( #7683, #9810 ) ) ;
#15169 = FACE_OUTER_BOUND ( 'NONE', #17102, .T. ) ;
#15170 = AXIS2_PLACEMENT_3D ( 'NONE', #14390, #7165, #18080 ) ;
#15171 = PERSON_AND_ORGANIZATION ( #11966, #8758 ) ;
#15172 = AXIS2_PLACEMENT_3D ( 'NONE', #5238, #12495, #19960 ) ;
#15173 = SECURITY_CLASSIFICATION_LEVEL ( 'unclassified' ) ;
#15174 = DIRECTION ( 'NONE',  ( -0.9730401042858024541, 0.2306359803922080898, 5.959266323858942451E-17 ) ) ;
#15175 = VECTOR ( 'NONE', #6072, 999.9999999999998863 ) ;
#15176 = CIRCLE ( 'NONE', #13286, 2.499999999999998668 ) ;
#15177 = DIRECTION ( 'NONE',  ( 0.000000000000000000, -1.000000000000000000, 5.035481788031372371E-15 ) ) ;
#15178 = ORIENTED_EDGE ( 'NONE', *, *, #3410, .F. ) ;
#15179 = APPLICATION_CONTEXT ( 'configuration controlled 3d designs of mechanical parts and assemblies' ) ;
#15180 = PERSON_AND_ORGANIZATION_ROLE ( 'design_supplier' ) ;
#15181 = EDGE_CURVE ( 'NONE', #10804, #16965, #13296, .T. ) ;
#15182 = PRODUCT ( 'F2', 'F2', '', ( #1709 ) ) ;
#15183 = CC_DESIGN_SECURITY_CLASSIFICATION ( #6084, ( #8383 ) ) ;
#15184 = ORIENTED_EDGE ( 'NONE', *, *, #3237, .F. ) ;
#15185 =( GEOMETRIC_REPRESENTATION_CONTEXT ( 3 ) GLOBAL_UNCERTAINTY_ASSIGNED_CONTEXT ( ( #3955 ) ) GLOBAL_UNIT_ASSIGNED_CONTEXT ( ( #5062, #4265, #6039 ) ) REPRESENTATION_CONTEXT ( 'NONE', 'WORKASPACE' ) );
#15186 = CARTESIAN_POINT ( 'NONE',  ( 35.75979881747886679, 26.94964815373086608, -13.00000000000049916 ) ) ;
#15187 = DIRECTION ( 'NONE',  ( 9.412241839989958199E-48, -1.000000000000000000, 2.441916418604790135E-15 ) ) ;
#15188 = EDGE_LOOP ( 'NONE', ( #1080, #22842, #2796, #9282 ) ) ;
#15189 = DIRECTION ( 'NONE',  ( 0.2306359803922076457, 0.9730401042858025651, 0.000000000000000000 ) ) ;
#15190 = DIRECTION ( 'NONE',  ( 1.213490492418610097E-15, 4.861311874477940294E-15, 1.000000000000000000 ) ) ;
#15191 = CARTESIAN_POINT ( 'NONE',  ( -19.99999999999809930, -20.00000000000000000, 8.500000000004551026 ) ) ;
#15192 = VERTEX_POINT ( 'NONE', #11418 ) ;
#15193 = ORIENTED_EDGE ( 'NONE', *, *, #17934, .F. ) ;
#15194 = DIRECTION ( 'NONE',  ( 0.7806762821593219437, -0.6249356306643899517, -1.759009604640482394E-13 ) ) ;
#15195 = ORIENTED_EDGE ( 'NONE', *, *, #20585, .F. ) ;
#15196 = VECTOR ( 'NONE', #7687, 1000.000000000000000 ) ;
#15197 = EDGE_CURVE ( 'NONE', #22534, #1573, #6124, .T. ) ;
#15198 = EDGE_CURVE ( 'NONE', #21456, #11668, #4274, .T. ) ;
#15199 = APPROVAL_STATUS ( 'not_yet_approved' ) ;
#15200 = ORIENTED_EDGE ( 'NONE', *, *, #5113, .T. ) ;
#15201 = VERTEX_POINT ( 'NONE', #21839 ) ;
#15202 = LINE ( 'NONE', #22443, #12298 ) ;
#15203 =( BOUNDED_CURVE ( )  B_SPLINE_CURVE ( 2, ( #22858, #6723, #21190 ),
 .UNSPECIFIED., .F., .F. ) 
 B_SPLINE_CURVE_WITH_KNOTS ( ( 3, 3 ),
 ( 0.08763271035584448143, 0.1752654207116860208 ),
 .UNSPECIFIED. ) 
 CURVE ( )  GEOMETRIC_REPRESENTATION_ITEM ( )  RATIONAL_B_SPLINE_CURVE ( ( 1.077350269189624843, 1.077350269189623511, 1.000000000000000000 ) ) 
 REPRESENTATION_ITEM ( '' )  );
#15204 = CALENDAR_DATE ( 2026, 31, 10 ) ;
#15205 = CLOSED_SHELL ( 'NONE', ( #1413, #10234, #7166, #10916 ) ) ;
#15206 = DIRECTION ( 'NONE',  ( -2.269700743865584947E-13, -2.220446049247695246E-15, -1.000000000000000000 ) ) ;
#15207 = APPROVAL_PERSON_ORGANIZATION ( #11178, #10855, #7578 ) ;
#15208 = FACE_OUTER_BOUND ( 'NONE', #9856, .T. ) ;
#15209 = APPROVAL_PERSON_ORGANIZATION ( #2109, #6932, #17063 ) ;
#15210 = VECTOR ( 'NONE', #12697, 1000.000000000000114 ) ;
#15211 =( LENGTH_UNIT ( ) NAMED_UNIT ( * ) SI_UNIT ( .MILLI., .METRE. ) );
#15212 = LOCAL_TIME ( 14, 11, 27.00000000000000000, #22643 ) ;
#15213 = CYLINDRICAL_SURFACE ( 'NONE', #11737, 2.999999999999999556 ) ;
#15214 = PERSON_AND_ORGANIZATION ( #11966, #8758 ) ;
#15215 = ADVANCED_FACE ( 'NONE', ( #12826 ), #20059, .F. ) ;
#15216 = ORIENTED_EDGE ( 'NONE', *, *, #23114, .T. ) ;
#15217 = CARTESIAN_POINT ( 'NONE',  ( 113.9197686726213448, -24.27486053345101169, -13.00000000000000000 ) ) ;
#15218 = DIRECTION ( 'NONE',  ( 0.000000000000000000, -1.000000000000000000, 0.000000000000000000 ) ) ;
#15219 = VERTEX_POINT ( 'NONE', #16494 ) ;
#15220 = EDGE_CURVE ( 'NONE', #15757, #12850, #8424, .T. ) ;
#15221 = CC_DESIGN_APPROVAL ( #778, ( #13725 ) ) ;
#15222 = CARTESIAN_POINT ( 'NONE',  ( 30.57814311865390167, -3.583136841839989817, 15.00000000000000000 ) ) ;
#15223 = CARTESIAN_POINT ( 'NONE',  ( -62.93889088200999282, 12.71096966728388722, -4.999999999999999112 ) ) ;
#15224 = LOCAL_TIME ( 14, 11, 27.00000000000000000, #19745 ) ;
#15225 = ORIENTED_EDGE ( 'NONE', *, *, #9439, .T. ) ;
#15226 = CARTESIAN_POINT ( 'NONE',  ( -25.00842861987479182, -15.87143667223269539, 21.49999999999999289 ) ) ;
#15227 = AXIS2_PLACEMENT_3D ( 'NONE', #8658, #3412, #19810 ) ;
#15228 = EDGE_CURVE ( 'NONE', #12528, #4039, #11460, .T. ) ;
#15229 = COORDINATED_UNIVERSAL_TIME_OFFSET ( 0, 0, .AHEAD. ) ;
#15231 = ADVANCED_FACE ( 'NONE', ( #15666 ), #11895, .T. ) ;
#15230 = VERTEX_POINT ( 'NONE', #6398 ) ;
#15232 = ORIENTED_EDGE ( 'NONE', *, *, #10248, .T. ) ;
#15233 = CARTESIAN_POINT ( 'NONE',  ( 120.8143550994449953, 2.935590694028619829, -13.00000000000000000 ) ) ;
#15234 = CC_DESIGN_APPROVAL ( #1209, ( #1966 ) ) ;
#15235 = ORIENTED_EDGE ( 'NONE', *, *, #850, .F. ) ;
#15236 = PERSON_AND_ORGANIZATION_ROLE ( 'design_owner' ) ;
#15237 = FACE_OUTER_BOUND ( 'NONE', #6167, .T. ) ;
#15238 = DIRECTION ( 'NONE',  ( 2.982858504577314686E-17, -2.441916418604790135E-15, -1.000000000000000000 ) ) ;
#15239 = CALENDAR_DATE ( 2026, 31, 10 ) ;
#15240 = CARTESIAN_POINT ( 'NONE',  ( -20.00000000000000000, -20.00000000000000000, 2.500000000000000000 ) ) ;
#15241 = LOCAL_TIME ( 14, 11, 27.00000000000000000, #8203 ) ;
#15242 =( NAMED_UNIT ( * ) PLANE_ANGLE_UNIT ( ) SI_UNIT ( $, .RADIAN. ) );
#15243 = AXIS2_PLACEMENT_3D ( 'NONE', #14179, #4914, #3008 ) ;
#15244 = DIRECTION ( 'NONE',  ( 0.7070970883417637687, 0.003702385528197202434, 0.7071067811865479058 ) ) ;
#15245 = PERSON_AND_ORGANIZATION ( #11966, #8758 ) ;
#15246 = CC_DESIGN_SECURITY_CLASSIFICATION ( #1966, ( #23503 ) ) ;
#15247 = DIRECTION ( 'NONE',  ( -0.9730401042858035643, 0.2306359803922028717, 5.432877459303547053E-17 ) ) ;
#15248 = CARTESIAN_POINT ( 'NONE',  ( 49.97703550743810297, 19.72589006658010291, 10.49999999999999822 ) ) ;
#15249 = CC_DESIGN_PERSON_AND_ORGANIZATION_ASSIGNMENT ( #17850, #5030, ( #5504 ) ) ;
#15250 = CARTESIAN_POINT ( 'NONE',  ( -65.80336369117380002, 8.448563927732790191, -5.000000000000000000 ) ) ;
#15251 = LINE ( 'NONE', #4093, #3080 ) ;
#15252 = CIRCLE ( 'NONE', #16010, 0.3999999999999998557 ) ;
#15253 = LINE ( 'NONE', #22499, #475 ) ;
#15254 = ORIENTED_EDGE ( 'NONE', *, *, #14065, .T. ) ;
#15255 = LOCAL_TIME ( 14, 11, 27.00000000000000000, #22056 ) ;
#15256 = VERTEX_POINT ( 'NONE', #20884 ) ;
#15257 = CARTESIAN_POINT ( 'NONE',  ( -65.82539143210260590, 12.65551411021120032, -5.000000000000000000 ) ) ;
#15258 = DIRECTION ( 'NONE',  ( 0.000000000000000000, -1.000000000000000000, 2.081668171172169697E-15 ) ) ;
#15259 = ORIENTED_EDGE ( 'NONE', *, *, #4735, .T. ) ;
#15260 = AXIS2_PLACEMENT_3D ( 'NONE', #2636, #15104, #4182 ) ;
#15261 = AXIS2_PLACEMENT_3D ( 'NONE', #6351, #11835, #14912 ) ;
#15262 = CARTESIAN_POINT ( 'NONE',  ( -19.99999998731729889, 20.45208919256890212, 4.459672832034550052E-12 ) ) ;
#15263 = ORIENTED_EDGE ( 'NONE', *, *, #18987, .T. ) ;
#15264 = CIRCLE ( 'NONE', #16002, 2.379999999999999893 ) ;
#15265 = CARTESIAN_POINT ( 'NONE',  ( 36.57467860885130051, 21.71590586959130320, -11.00000000000049916 ) ) ;
#15266 = COORDINATED_UNIVERSAL_TIME_OFFSET ( 0, 0, .AHEAD. ) ;
#15267 = CARTESIAN_POINT ( 'NONE',  ( -20.00000000397400157, 22.95208919257349933, -5.499999999995569766 ) ) ;
#15268 = CIRCLE ( 'NONE', #20188, 2.501000000000000334 ) ;
#15269 = EDGE_CURVE ( 'NONE', #5418, #5938, #18669, .T. ) ;
#15270 = DATE_AND_TIME ( #2682, #16378 ) ;
#15271 = CIRCLE ( 'NONE', #11508, 2.500000000000000000 ) ;
#15273 = AXIS2_PLACEMENT_3D ( 'NONE', #13875, #3407, #14105 ) ;
#15272 = CARTESIAN_POINT ( 'NONE',  ( 37.88245768368250310, -4.127756955731490152, 13.00000000000000000 ) ) ;
#15274 = LOCAL_TIME ( 14, 11, 27.00000000000000000, #6390 ) ;
#15275 = CARTESIAN_POINT ( 'NONE',  ( -19.49999999982360066, -0.1021026942259749964, -2.500000000000000000 ) ) ;
#15276 = ORIENTED_EDGE ( 'NONE', *, *, #16872, .T. ) ;
#15277 = DIRECTION ( 'NONE',  ( -1.000000000000000000, 2.270069654138870255E-15, 0.000000000000000000 ) ) ;
#15278 = AXIS2_PLACEMENT_3D ( 'NONE', #18459, #22118, #724 ) ;
#15279 = AXIS2_PLACEMENT_3D ( 'NONE', #6118, #6246, #993 ) ;
#15280 = CYLINDRICAL_SURFACE ( 'NONE', #11819, 2.500000000000000444 ) ;
#15281 = ORIENTED_EDGE ( 'NONE', *, *, #11620, .T. ) ;
#15282 = DIRECTION ( 'NONE',  ( 0.000000000000000000, 0.000000000000000000, -1.000000000000000000 ) ) ;
#15283 = CARTESIAN_POINT ( 'NONE',  ( 115.1780992045983680, -12.17177901375979410, 3.431286017404439083E-14 ) ) ;
#15284 = UNCERTAINTY_MEASURE_WITH_UNIT (LENGTH_MEASURE( 1.000000000000000082E-05 ), #8516, 'distance_accuracy_value', 'NONE');
#15285 = APPROVAL_STATUS ( 'not_yet_approved' ) ;
#15286 = DIRECTION ( 'NONE',  ( 0.000000000000000000, 0.000000000000000000, -1.000000000000000000 ) ) ;
#15287 = AXIS2_PLACEMENT_3D ( 'NONE', #10534, #3158, #4933 ) ;
#15288 = ORIENTED_EDGE ( 'NONE', *, *, #2822, .T. ) ;
#15289 = VECTOR ( 'NONE', #6872, 1000.000000000000114 ) ;
#15290 = MECHANICAL_CONTEXT ( 'NONE', #8680, 'mechanical' ) ;
#15291 = CARTESIAN_POINT ( 'NONE',  ( -27.00000000000000000, -31.09999999999999787, 21.50000000000000000 ) ) ;
#15292 = SECURITY_CLASSIFICATION ( '', '', #1237 ) ;
#15293 = ORIENTED_EDGE ( 'NONE', *, *, #5223, .T. ) ;
#15294 = ORIENTED_EDGE ( 'NONE', *, *, #11189, .T. ) ;
#15295 = CALENDAR_DATE ( 2026, 31, 10 ) ;
#15296 = VECTOR ( 'NONE', #4889, 1000.000000000000000 ) ;
#15297 = AXIS2_PLACEMENT_3D ( 'NONE', #4535, #17727, #17263 ) ;
#15298 = EDGE_CURVE ( 'NONE', #19671, #11858, #13879, .T. ) ;
#15299 = VECTOR ( 'NONE', #13230, 1000.000000000000000 ) ;
#15300 = DATE_AND_TIME ( #22413, #15212 ) ;
#15301 = DIRECTION ( 'NONE',  ( 0.6660003063074656504, -0.7459514675891198987, 0.000000000000000000 ) ) ;
#15302 = APPROVAL ( #22750, 'UNKNOWN' ) ;
#15304 = AXIS2_PLACEMENT_3D ( 'NONE', #23051, #5014, #14036 ) ;
#15303 = CARTESIAN_POINT ( 'NONE',  ( 122.4288069621910040, 9.746871424029270869, 10.02499999999999858 ) ) ;
#15305 = ORIENTED_EDGE ( 'NONE', *, *, #5873, .T. ) ;
#15306 = EDGE_CURVE ( 'NONE', #3681, #7436, #14094, .T. ) ;
#15307 = ADVANCED_FACE ( 'NONE', ( #13642 ), #804, .T. ) ;
#15308 = PERSON_AND_ORGANIZATION_ROLE ( 'design_supplier' ) ;
#15309 = CIRCLE ( 'NONE', #6216, 2.500000000000000000 ) ;
#15310 = ORIENTED_EDGE ( 'NONE', *, *, #17683, .T. ) ;
#15311 = AXIS2_PLACEMENT_3D ( 'NONE', #5575, #9149, #2372 ) ;
#15312 = CARTESIAN_POINT ( 'NONE',  ( 36.84099409957980242, 22.83947580187480142, 13.00000000000000000 ) ) ;
#15313 = PLANE ( 'NONE',  #629 ) ;
#15314 = ORIENTED_EDGE ( 'NONE', *, *, #4086, .F. ) ;
#15315 = CARTESIAN_POINT ( 'NONE',  ( -14.54830929662709949, 0.3367883020382470560, 8.000000000004449774 ) ) ;
#15316 = CARTESIAN_POINT ( 'NONE',  ( 2.499999999999970246, -30.47499999999999787, 19.00000000000000000 ) ) ;
#15317 = CARTESIAN_POINT ( 'NONE',  ( 35.34725016111838869, 18.05499787358298036, -13.00000000000030020 ) ) ;
#15318 = EDGE_LOOP ( 'NONE', ( #21129, #19413, #2133, #10193 ) ) ;
#15319 = EDGE_LOOP ( 'NONE', ( #14957, #10798, #18442, #19211 ) ) ;
#15320 = LINE ( 'NONE', #10346, #11025 ) ;
#15321 = EDGE_LOOP ( 'NONE', ( #6184, #7569, #8694, #373, #21844 ) ) ;
#15322 = APPROVAL_STATUS ( 'not_yet_approved' ) ;
#15323 = ORIENTED_EDGE ( 'NONE', *, *, #7083, .T. ) ;
#15324 = ORIENTED_EDGE ( 'NONE', *, *, #14739, .T. ) ;
#15325 = CARTESIAN_POINT ( 'NONE',  ( 11.50000000000000000, -23.36217782649120167, 2.500000000000000000 ) ) ;
#15326 = PERSON_AND_ORGANIZATION ( #11966, #8758 ) ;
#15327 = EDGE_CURVE ( 'NONE', #15708, #12824, #22655, .T. ) ;
#15328 = CIRCLE ( 'NONE', #8135, 4.349999999999996980 ) ;
#15329 = DIRECTION ( 'NONE',  ( -2.882701132343535037E-16, -9.096985413436440085E-33, 1.000000000000000000 ) ) ;
#15330 = AXIS2_PLACEMENT_3D ( 'NONE', #19816, #3074, #5102 ) ;
#15331 = CC_DESIGN_PERSON_AND_ORGANIZATION_ASSIGNMENT ( #10353, #17593, ( #8185 ) ) ;
#15332 = CC_DESIGN_PERSON_AND_ORGANIZATION_ASSIGNMENT ( #1297, #197, ( #21217 ) ) ;
#15333 = EDGE_CURVE ( 'NONE', #20293, #17804, #19923, .T. ) ;
#15334 = EDGE_CURVE ( 'NONE', #19340, #16530, #16742, .T. ) ;
#15335 = CARTESIAN_POINT ( 'NONE',  ( -58.60882321939752160, 12.73364205572179841, -2.499999999999991118 ) ) ;
#15336 = PERSON_AND_ORGANIZATION ( #11966, #8758 ) ;
#15337 = APPROVAL ( #9675, 'UNSPECIFIED' ) ;
#15338 = VERTEX_POINT ( 'NONE', #2842 ) ;
#15339 = CARTESIAN_POINT ( 'NONE',  ( -69.91240388362379576, 7.634045827809354812, -7.200000000000000178 ) ) ;
#15340 = CARTESIAN_POINT ( 'NONE',  ( 114.1489752661110089, -25.18526831983109915, -3.000000000000000000 ) ) ;
#15341 = EDGE_LOOP ( 'NONE', ( #14354, #1985, #21707, #942 ) ) ;
#15342 = DIRECTION ( 'NONE',  ( 0.000000000000000000, 0.000000000000000000, 1.000000000000000000 ) ) ;
#15343 = CARTESIAN_POINT ( 'NONE',  ( -18.05391955182270181, 22.49081825942809942, -4.900728725074969882E-15 ) ) ;
#15344 = ORIENTED_EDGE ( 'NONE', *, *, #4874, .T. ) ;
#15345 = DIRECTION ( 'NONE',  ( -1.000000000000000000, -6.662111140531837817E-09, 1.144917494144693313E-14 ) ) ;
#15346 = PERSON_AND_ORGANIZATION ( #11966, #8758 ) ;
#15347 = VERTEX_POINT ( 'NONE', #17332 ) ;
#15348 = ORIENTED_EDGE ( 'NONE', *, *, #1613, .F. ) ;
#15349 = DIRECTION ( 'NONE',  ( -3.099353312215989243E-62, 1.308200680535015858E-77, 1.000000000000000000 ) ) ;
#15350 = DIRECTION ( 'NONE',  ( -0.9730401042858035643, 0.2306359803922028717, 5.958148513035547083E-17 ) ) ;
#15351 = ORIENTED_EDGE ( 'NONE', *, *, #5873, .F. ) ;
#15352 = PERSON_AND_ORGANIZATION_ROLE ( 'design_owner' ) ;
#15353 = FACE_OUTER_BOUND ( 'NONE', #14114, .T. ) ;
#15354 = EDGE_CURVE ( 'NONE', #22529, #90, #6512, .T. ) ;
#15355 = DIRECTION ( 'NONE',  ( -3.210834492181045054E-17, 2.441916418604790135E-15, 1.000000000000000000 ) ) ;
#15356 = ITEM_DEFINED_TRANSFORMATION ( 'NONE', 'NONE', #12538,  #12739 ) ;
#15357 = CARTESIAN_POINT ( 'NONE',  ( -19.49999999982379961, -0.1021026942259709996, 9.160072195675308484E-14 ) ) ;
#15358 = EDGE_CURVE ( 'NONE', #4836, #5730, #15536, .T. ) ;
#15359 = VECTOR ( 'NONE', #11649, 1000.000000000000114 ) ;
#15360 = ADVANCED_FACE ( 'NONE', ( #19337 ), #3089, .F. ) ;
#15361 = DIRECTION ( 'NONE',  ( 0.9999862922474491711, 0.005235963827116866913, -1.514467536079854800E-31 ) ) ;
#15362 = PERSON_AND_ORGANIZATION ( #11966, #8758 ) ;
#15363 = EDGE_CURVE ( 'NONE', #1299, #1783, #1942, .T. ) ;
#15364 = FACE_OUTER_BOUND ( 'NONE', #1582, .T. ) ;
#15365 = LINE ( 'NONE', #10162, #14285 ) ;
#15366 = DIRECTION ( 'NONE',  ( -1.164423685541410132E-14, -4.938475812832940103E-14, 1.000000000000000000 ) ) ;
#15367 = DIRECTION ( 'NONE',  ( -2.065223582182029992E-34, 2.636263576915770120E-16, -1.000000000000000000 ) ) ;
#15368 = FACE_OUTER_BOUND ( 'NONE', #12493, .T. ) ;
#15369 = DIRECTION ( 'NONE',  ( -3.210834492181045054E-17, 2.441916418604790135E-15, 1.000000000000000000 ) ) ;
#15370 = ORIENTED_EDGE ( 'NONE', *, *, #19680, .F. ) ;
#15371 = CIRCLE ( 'NONE', #9311, 7.000000000000000000 ) ;
#15372 = ORIENTED_EDGE ( 'NONE', *, *, #11986, .T. ) ;
#15373 = CARTESIAN_POINT ( 'NONE',  ( -21.66385406723090057, 11.15564796089419985, 5.000000000000000000 ) ) ;
#15374 = CARTESIAN_POINT ( 'NONE',  ( 114.9904400984930106, 13.05151942359559847, 2.909781424016149503E-14 ) ) ;
#15375 = ORIENTED_EDGE ( 'NONE', *, *, #20360, .T. ) ;
#15376 = CARTESIAN_POINT ( 'NONE',  ( 5.000000000000000000, -31.09999999999999787, -2.500000000000000000 ) ) ;
#15377 = ORIENTED_EDGE ( 'NONE', *, *, #10403, .T. ) ;
#15378 = CARTESIAN_POINT ( 'NONE',  ( -62.93786153767959490, 12.51438117767279934, 2.729132938682643950 ) ) ;
#15379 = DATE_AND_TIME ( #8153, #859 ) ;
#15380 = CARTESIAN_POINT ( 'NONE',  ( -32.64674982798959491, 7.329300507370480666, 3.750000000000000000 ) ) ;
#15381 = PRODUCT_DEFINITION_SHAPE ( 'NONE', 'NONE',  #17062 ) ;
#15382 = APPROVAL_DATE_TIME ( #2916, #2380 ) ;
#15383 = EDGE_CURVE ( 'NONE', #15757, #9430, #7954, .T. ) ;
#15384 = DIRECTION ( 'NONE',  ( 1.138590270679734009E-14, 2.220446049251240387E-15, 1.000000000000000000 ) ) ;
#15385 = CARTESIAN_POINT ( 'NONE',  ( 26.11627841292215280, -8.532812502301730717, -16.00000000000000000 ) ) ;
#15386 = AXIS2_PLACEMENT_3D ( 'NONE', #19871, #14044, #21624 ) ;
#15387 = CARTESIAN_POINT ( 'NONE',  ( -20.00000000000000000, -20.00000000000000000, 2.500000000000000000 ) ) ;
#15388 = EDGE_LOOP ( 'NONE', ( #3427, #8953 ) ) ;
#15389 = CARTESIAN_POINT ( 'NONE',  ( 84.26187758838335640, -12.29469986460243724, -13.00000000000000000 ) ) ;
#15390 = AXIS2_PLACEMENT_3D ( 'NONE', #1598, #10654, #17882 ) ;
#15391 = DIRECTION ( 'NONE',  ( -1.466984912809907930E-16, -2.805478249466190329E-20, -1.000000000000000000 ) ) ;
#15392 = VERTEX_POINT ( 'NONE', #2724 ) ;
#15393 = CARTESIAN_POINT ( 'NONE',  ( 112.4091670724712060, 2.161275108032480130, 3.197661755011519713E-14 ) ) ;
#15394 = DIRECTION ( 'NONE',  ( 2.270069654138865127E-15, 1.000000000000000000, 4.574083617919690056E-30 ) ) ;
#15395 = EDGE_CURVE ( 'NONE', #6910, #23250, #6169, .T. ) ;
#15396 = APPROVAL_DATE_TIME ( #13623, #921 ) ;
#15397 = FACE_OUTER_BOUND ( 'NONE', #3411, .T. ) ;
#15398 = ORIENTED_EDGE ( 'NONE', *, *, #6152, .F. ) ;
#15399 = ORIENTED_EDGE ( 'NONE', *, *, #15469, .T. ) ;
#15400 = COORDINATED_UNIVERSAL_TIME_OFFSET ( 0, 0, .AHEAD. ) ;
#15401 = DIRECTION ( 'NONE',  ( 1.000000000000000000, -2.270069654138870255E-15, 3.099353312215988811E-62 ) ) ;
#15402 = EDGE_LOOP ( 'NONE', ( #18899, #18844, #12569, #20220 ) ) ;
#15403 = ORIENTED_EDGE ( 'NONE', *, *, #5747, .F. ) ;
#15404 = CARTESIAN_POINT ( 'NONE',  ( -19.49999999982360066, -0.1021026942259700004, 2.500000000000000000 ) ) ;
#15405 = APPROVAL_STATUS ( 'not_yet_approved' ) ;
#15406 = CALENDAR_DATE ( 2026, 31, 10 ) ;
#15407 = PLANE ( 'NONE',  #8161 ) ;
#15408 = DIRECTION ( 'NONE',  ( 0.9822610636820822139, -0.1875185398144529336, 5.059610138265687687E-16 ) ) ;
#15409 = ORIENTED_EDGE ( 'NONE', *, *, #13866, .T. ) ;
#15410 = PERSON_AND_ORGANIZATION_ROLE ( 'design_owner' ) ;
#15411 = AXIS2_PLACEMENT_3D ( 'NONE', #8632, #10078, #5073 ) ;
#15412 = AXIS2_PLACEMENT_3D ( 'NONE', #12178, #11827, #15482 ) ;
#15413 = CIRCLE ( 'NONE', #3669, 2.749999999999999112 ) ;
#15414 = ORIENTED_EDGE ( 'NONE', *, *, #12191, .T. ) ;
#15415 = CARTESIAN_POINT ( 'NONE',  ( -26.00000000397269773, 22.95208919201850151, 6.750000000004529710 ) ) ;
#15416 = DIRECTION ( 'NONE',  ( 0.1630842657209383706, 0.6880432561069579345, 0.7071067811865456854 ) ) ;
#15418 = VERTEX_POINT ( 'NONE', #16006 ) ;
#15417 = ADVANCED_FACE ( 'NONE', ( #20653 ), #5373, .F. ) ;
#15419 = EDGE_CURVE ( 'NONE', #18309, #15573, #10573, .T. ) ;
#15420 = DIRECTION ( 'NONE',  ( 6.124378941434239724E-17, -2.274246353359159970E-33, 1.000000000000000000 ) ) ;
#15421 = DIRECTION ( 'NONE',  ( 1.138590270679734009E-14, 2.220446049251240387E-15, 1.000000000000000000 ) ) ;
#15422 = FACE_OUTER_BOUND ( 'NONE', #532, .T. ) ;
#15423 = ORIENTED_EDGE ( 'NONE', *, *, #15269, .F. ) ;
#15424 = VERTEX_POINT ( 'NONE', #1743 ) ;
#15425 = DIRECTION ( 'NONE',  ( 0.2306359803922089224, 0.9730401042858022320, -4.744007713284279563E-15 ) ) ;
#15426 = ORIENTED_EDGE ( 'NONE', *, *, #1498, .F. ) ;
#15427 = CC_DESIGN_PERSON_AND_ORGANIZATION_ASSIGNMENT ( #4597, #17311, ( #1214 ) ) ;
#15428 = MECHANICAL_CONTEXT ( 'NONE', #10667, 'mechanical' ) ;
#15429 = ORIENTED_EDGE ( 'NONE', *, *, #1133, .T. ) ;
#15430 = ORIENTED_EDGE ( 'NONE', *, *, #10974, .F. ) ;
#15431 = DIRECTION ( 'NONE',  ( 0.9730401042858035643, -0.2306359803922028717, -5.432877459303547053E-17 ) ) ;
#15432 = AXIS2_PLACEMENT_3D ( 'NONE', #9062, #12641, #14 ) ;
#15433 = COORDINATED_UNIVERSAL_TIME_OFFSET ( 0, 0, .AHEAD. ) ;
#15434 = EDGE_CURVE ( 'NONE', #4745, #2335, #15888, .T. ) ;
#15435 = EDGE_CURVE ( 'NONE', #2588, #9648, #17892, .T. ) ;
#15436 = VECTOR ( 'NONE', #20963, 1000.000000000000000 ) ;
#15437 = CARTESIAN_POINT ( 'NONE',  ( 34.14207834813670672, 22.29249582057180135, -15.00000000000049916 ) ) ;
#15438 = AXIS2_PLACEMENT_3D ( 'NONE', #17952, #3575, #1660 ) ;
#15439 = ADVANCED_FACE ( 'NONE', ( #18034 ), #5098, .T. ) ;
#15440 = AXIS2_PLACEMENT_3D ( 'NONE', #11235, #11353, #18704 ) ;
#15441 = LINE ( 'NONE', #22675, #695 ) ;
#15442 = DATE_AND_TIME ( #9886, #1941 ) ;
#15443 = ORIENTED_EDGE ( 'NONE', *, *, #32, .F. ) ;
#15444 = AXIS2_PLACEMENT_3D ( 'NONE', #3677, #23383, #10953 ) ;
#15445 = CARTESIAN_POINT ( 'NONE',  ( -14.00000000000000000, -19.99999999944489915, 8.000000000004488854 ) ) ;
#15446 = CARTESIAN_POINT ( 'NONE',  ( -25.00842861987479893, -15.87143667223269894, 23.00000000000000000 ) ) ;
#15447 = ORIENTED_EDGE ( 'NONE', *, *, #13329, .T. ) ;
#15448 = CIRCLE ( 'NONE', #13556, 0.5000000000000004441 ) ;
#15449 = EDGE_CURVE ( 'NONE', #11681, #12948, #4992, .T. ) ;
#15450 = VECTOR ( 'NONE', #14546, 1000.000000000000227 ) ;
#15451 = DIRECTION ( 'NONE',  ( 0.9949874374308176339, 0.09999999677427344469, -2.262079412673755946E-13 ) ) ;
#15452 = AXIS2_PLACEMENT_3D ( 'NONE', #9318, #10398, #6586 ) ;
#15453 = CARTESIAN_POINT ( 'NONE',  ( 39.27359436029429673, 22.26288585089429972, 8.749999999999998224 ) ) ;
#15454 = EDGE_LOOP ( 'NONE', ( #2698, #14578 ) ) ;
#15455 = CARTESIAN_POINT ( 'NONE',  ( 117.8160873543469904, -9.713930661686799084, 3.415130773183659557E-14 ) ) ;
#15456 = PRODUCT_RELATED_PRODUCT_CATEGORY ( 'detail', '', ( #15182 ) ) ;
#15457 = COORDINATED_UNIVERSAL_TIME_OFFSET ( 0, 0, .AHEAD. ) ;
#15458 = ORIENTED_EDGE ( 'NONE', *, *, #1340, .T. ) ;
#15459 = PRODUCT_DEFINITION ( 'UNKNOWN', '', #10349, #6849 ) ;
#15460 = ORIENTED_EDGE ( 'NONE', *, *, #3000, .F. ) ;
#15461 = CYLINDRICAL_SURFACE ( 'NONE', #5068, 3.499999999999998224 ) ;
#15462 = CARTESIAN_POINT ( 'NONE',  ( 36.76586756491560237, 21.07724224331881047, -12.00000000000050093 ) ) ;
#15463 = EDGE_LOOP ( 'NONE', ( #18384, #9470, #10765, #6427 ) ) ;
#15464 = VECTOR ( 'NONE', #8890, 1000.000000000000000 ) ;
#15465 = SECURITY_CLASSIFICATION_LEVEL ( 'unclassified' ) ;
#15466 = ADVANCED_FACE ( 'NONE', ( #10927 ), #8032, .T. ) ;
#15467 = DIRECTION ( 'NONE',  ( 2.982858504489139758E-17, -2.441916418604790135E-15, -1.000000000000000000 ) ) ;
#15468 = EDGE_CURVE ( 'NONE', #19182, #17821, #7274, .T. ) ;
#15469 = EDGE_CURVE ( 'NONE', #23382, #3254, #16242, .T. ) ;
#15470 = DIRECTION ( 'NONE',  ( 1.227507208848341976E-15, 4.920447605136010024E-15, 1.000000000000000000 ) ) ;
#15471 = AXIS2_PLACEMENT_3D ( 'NONE', #21120, #6523, #8428 ) ;
#15472 = DATE_AND_TIME ( #18929, #14765 ) ;
#15473 = DIRECTION ( 'NONE',  ( -1.000000000000000000, 2.270069654138870255E-15, -3.099353312215989243E-62 ) ) ;
#15474 = VECTOR ( 'NONE', #22011, 1000.000000000000000 ) ;
#15475 = AXIS2_PLACEMENT_3D ( 'NONE', #5985, #7772, #17021 ) ;
#15476 =( NAMED_UNIT ( * ) PLANE_ANGLE_UNIT ( ) SI_UNIT ( $, .RADIAN. ) );
#15477 = CARTESIAN_POINT ( 'NONE',  ( 114.0804991654443796, -24.53545640578393261, -13.00000000000000000 ) ) ;
#15478 = PERSON_AND_ORGANIZATION ( #11966, #8758 ) ;
#15479 =( BOUNDED_CURVE ( )  B_SPLINE_CURVE ( 2, ( #21545, #12776, #22014 ),
 .UNSPECIFIED., .F., .F. ) 
 B_SPLINE_CURVE_WITH_KNOTS ( ( 3, 3 ),
 ( 0.1168436138077985215, 0.2336872276155859962 ),
 .UNSPECIFIED. ) 
 CURVE ( )  GEOMETRIC_REPRESENTATION_ITEM ( )  RATIONAL_B_SPLINE_CURVE ( ( 1.077350269189629950, 1.077350269189626175, 1.000000000000000000 ) ) 
 REPRESENTATION_ITEM ( '' )  );
#15480 = CARTESIAN_POINT ( 'NONE',  ( 37.63682253917825449, 9.430584805299272233, 8.999987531128503804 ) ) ;
#15481 = DIRECTION ( 'NONE',  ( -0.9080618652418041004, 0.4188360644614733674, -1.040834085574019418E-15 ) ) ;
#15482 = DIRECTION ( 'NONE',  ( -0.2306359803922077290, -0.9730401042858024541, 0.000000000000000000 ) ) ;
#15483 = EDGE_CURVE ( 'NONE', #1999, #3328, #20528, .T. ) ;
#15484 = DIRECTION ( 'NONE',  ( 0.005235963827117002221, -0.9999862922474493931, -2.636227439667000721E-16 ) ) ;
#15486 = AXIS2_PLACEMENT_3D ( 'NONE', #12204, #22972, #17530 ) ;
#15485 = DIRECTION ( 'NONE',  ( 0.000000000000000000, 0.000000000000000000, -1.000000000000000000 ) ) ;
#15487 = CARTESIAN_POINT ( 'NONE',  ( -28.52462712253550237, 6.350733138482030249, 0.7325259402521709928 ) ) ;
#15488 = ORIENTED_EDGE ( 'NONE', *, *, #21592, .F. ) ;
#15489 = VERTEX_POINT ( 'NONE', #12238 ) ;
#15490 = LINE ( 'NONE', #10170, #3122 ) ;
#15491 = AXIS2_PLACEMENT_3D ( 'NONE', #13095, #4172, #11572 ) ;
#15492 = FACE_OUTER_BOUND ( 'NONE', #23118, .T. ) ;
#15493 = ORIENTED_EDGE ( 'NONE', *, *, #16143, .F. ) ;
#15494 = EDGE_CURVE ( 'NONE', #13437, #3681, #19929, .T. ) ;
#15495 = CARTESIAN_POINT ( 'NONE',  ( 58.73439644601037912, 17.65016624305025061, 10.99076000000003361 ) ) ;
#15496 = EDGE_CURVE ( 'NONE', #21863, #8039, #6766, .T. ) ;
#15497 = VERTEX_POINT ( 'NONE', #14112 ) ;
#15498 = DIRECTION ( 'NONE',  ( 6.124378941434239724E-17, -2.274246353359159970E-33, 1.000000000000000000 ) ) ;
#15499 = PERSON_AND_ORGANIZATION_ROLE ( 'classification_officer' ) ;
#15500 = LINE ( 'NONE', #8382, #14282 ) ;
#15501 = APPLICATION_CONTEXT ( 'configuration controlled 3d designs of mechanical parts and assemblies' ) ;
#15502 = COORDINATED_UNIVERSAL_TIME_OFFSET ( 0, 0, .AHEAD. ) ;
#15503 = FACE_OUTER_BOUND ( 'NONE', #19294, .T. ) ;
#15504 = CARTESIAN_POINT ( 'NONE',  ( -26.99999999999959854, -30.09999999999999787, 25.00000000000000000 ) ) ;
#15505 = CARTESIAN_POINT ( 'NONE',  ( 0.000000000000000000, 0.000000000000000000, 0.000000000000000000 ) ) ;
#15506 = CLOSED_SHELL ( 'NONE', ( #9420, #19309, #7043, #20403, #21568, #19371 ) ) ;
#15507 = DIRECTION ( 'NONE',  ( -1.000000000000000000, -6.662111140531837817E-09, 1.144917494144693313E-14 ) ) ;
#15508 = VERTEX_POINT ( 'NONE', #17688 ) ;
#15509 = DIRECTION ( 'NONE',  ( -1.000000000000000000, -6.662111140531837817E-09, 1.110223024625157172E-14 ) ) ;
#15510 = ADVANCED_FACE ( 'NONE', ( #21358 ), #21692, .T. ) ;
#15511 = DIRECTION ( 'NONE',  ( 5.798605125234323991E-17, -1.374421231021384554E-17, 1.000000000000000000 ) ) ;
#15512 = VERTEX_POINT ( 'NONE', #3303 ) ;
#15513 = CARTESIAN_POINT ( 'NONE',  ( 35.59419854219520118, 9.774809681453278998, -26.88000000000049994 ) ) ;
#15514 = AXIS2_PLACEMENT_3D ( 'NONE', #13246, #13713, #13598 ) ;
#15515 = CARTESIAN_POINT ( 'NONE',  ( -30.79177721110609767, 6.338862259904598950, 2.999707106781169585 ) ) ;
#15516 = DATE_TIME_ROLE ( 'classification_date' ) ;
#15517 = DIRECTION ( 'NONE',  ( 0.000000000000000000, 0.000000000000000000, -1.000000000000000000 ) ) ;
#15518 = VERTEX_POINT ( 'NONE', #23248 ) ;
#15519 = ORIENTED_EDGE ( 'NONE', *, *, #4469, .T. ) ;
#15520 = EDGE_CURVE ( 'NONE', #13437, #22247, #14463, .T. ) ;
#15521 = APPROVAL_DATE_TIME ( #20750, #14012 ) ;
#15522 = DIRECTION ( 'NONE',  ( -1.000000000000000000, 0.000000000000000000, 0.000000000000000000 ) ) ;
#15523 = EDGE_LOOP ( 'NONE', ( #14239, #11562 ) ) ;
#15524 = EDGE_CURVE ( 'NONE', #5709, #10223, #17916, .T. ) ;
#15525 = DIRECTION ( 'NONE',  ( -0.9999862922474491711, -0.005235963827128305680, 1.734723475976808327E-16 ) ) ;
#15526 = APPROVAL_ROLE ( '' ) ;
#15527 = PRODUCT ( 'Pin 2', 'Pin 2', '', ( #6516 ) ) ;
#15528 = ITEM_DEFINED_TRANSFORMATION ( 'NONE', 'NONE', #3058,  #12739 ) ;
#15529 = CARTESIAN_POINT ( 'NONE',  ( 34.40556712239430226, 8.514986143071238800, 29.25000000000000000 ) ) ;
#15530 = LOCAL_TIME ( 14, 11, 27.00000000000000000, #11187 ) ;
#15531 = AXIS2_PLACEMENT_3D ( 'NONE', #11106, #18460, #18099 ) ;
#15532 = DIRECTION ( 'NONE',  ( 0.000000000000000000, 0.000000000000000000, -1.000000000000000000 ) ) ;
#15533 = VERTEX_POINT ( 'NONE', #23006 ) ;
#15534 = PERSON_AND_ORGANIZATION_ROLE ( 'classification_officer' ) ;
#15535 = VERTEX_POINT ( 'NONE', #23355 ) ;
#15536 = LINE ( 'NONE', #3069, #9560 ) ;
#15537 = LINE ( 'NONE', #19228, #6710 ) ;
#15538 = VERTEX_POINT ( 'NONE', #10809 ) ;
#15539 = CC_DESIGN_DATE_AND_TIME_ASSIGNMENT ( #5954, #2043, ( #19756 ) ) ;
#15540 = CYLINDRICAL_SURFACE ( 'NONE', #10950, 4.750000000000000000 ) ;
#15541 = CARTESIAN_POINT ( 'NONE',  ( 39.69419854219519550, 9.774809681453278998, -25.00000000000000000 ) ) ;
#15542 = DIRECTION ( 'NONE',  ( -0.9730401042858036753, 0.2306359803922028995, 5.959266323858677443E-17 ) ) ;
#15543 = CIRCLE ( 'NONE', #16301, 8.250000000000000000 ) ;
#15544 = ORIENTED_EDGE ( 'NONE', *, *, #12055, .T. ) ;
#15545 = AXIS2_PLACEMENT_3D ( 'NONE', #8448, #20673, #4518 ) ;
#15546 = ORIENTED_EDGE ( 'NONE', *, *, #16881, .T. ) ;
#15548 = AXIS2_PLACEMENT_3D ( 'NONE', #19854, #10844, #1776 ) ;
#15547 = LINE ( 'NONE', #22783, #1124 ) ;
#15549 = ORIENTED_EDGE ( 'NONE', *, *, #5316, .F. ) ;
#15550 = PERSON_AND_ORGANIZATION ( #11966, #8758 ) ;
#15551 = ORIENTED_EDGE ( 'NONE', *, *, #3541, .F. ) ;
#15552 = VERTEX_POINT ( 'NONE', #7117 ) ;
#15553 = DIRECTION ( 'NONE',  ( 0.9730401042858036753, -0.2306359803922028995, -3.393930153960344319E-16 ) ) ;
#15554 = PERSON_AND_ORGANIZATION ( #11966, #8758 ) ;
#15555 = VECTOR ( 'NONE', #13325, 999.9999999999998863 ) ;
#15556 = CARTESIAN_POINT ( 'NONE',  ( 40.45939906362549721, 8.621629779493760637, 3.888892445930440142E-14 ) ) ;
#15557 = ADVANCED_FACE ( 'NONE', ( #21576 ), #5313, .T. ) ;
#15558 = APPROVAL_PERSON_ORGANIZATION ( #5966, #15337, #18918 ) ;
#15559 = DIRECTION ( 'NONE',  ( 1.000000000000000000, 0.000000000000000000, 0.000000000000000000 ) ) ;
#15560 = CARTESIAN_POINT ( 'NONE',  ( 35.59419854219520118, 9.774809681453540122, 26.30000000000000071 ) ) ;
#15561 = AXIS2_PLACEMENT_3D ( 'NONE', #5763, #13024, #1403 ) ;
#15562 = DIRECTION ( 'NONE',  ( -0.9730401042858022320, 0.2306359803922080343, 5.959266323858941219E-17 ) ) ;
#15563 = APPROVAL_ROLE ( '' ) ;
#15564 = ORIENTED_EDGE ( 'NONE', *, *, #15524, .T. ) ;
#15565 = DIRECTION ( 'NONE',  ( -0.2306359803922090335, -0.9730401042858022320, 4.744007713284281141E-15 ) ) ;
#15566 = LINE ( 'NONE', #11684, #16575 ) ;
#15567 = CIRCLE ( 'NONE', #20152, 3.499999999999998224 ) ;
#15568 = ORIENTED_EDGE ( 'NONE', *, *, #16966, .T. ) ;
#15569 = ADVANCED_FACE ( 'NONE', ( #18940 ), #55, .T. ) ;
#15570 = DIRECTION ( 'NONE',  ( 0.2306359803922080898, 0.9730401042858024541, -2.572202231434325988E-16 ) ) ;
#15571 = CARTESIAN_POINT ( 'NONE',  ( -12.59661859122890171, -1.225550774622820027, 6.750000000004429346 ) ) ;
#15572 = CARTESIAN_POINT ( 'NONE',  ( -26.99999999999959854, 8.392275869980100359E-122, 21.49999999999999289 ) ) ;
#15573 = VERTEX_POINT ( 'NONE', #22042 ) ;
#15574 = CARTESIAN_POINT ( 'NONE',  ( -69.82562477157480885, -8.939392295122029708, -7.200000000000000178 ) ) ;
#15575 = COORDINATED_UNIVERSAL_TIME_OFFSET ( 0, 0, .AHEAD. ) ;
#15576 = CC_DESIGN_SECURITY_CLASSIFICATION ( #14054, ( #7614 ) ) ;
#15577 = ORIENTED_EDGE ( 'NONE', *, *, #11122, .T. ) ;
#15578 = ORIENTED_EDGE ( 'NONE', *, *, #22563, .F. ) ;
#15579 = DIRECTION ( 'NONE',  ( -0.2306359803922080898, -0.9730401042858024541, 2.572202231434325988E-16 ) ) ;
#15580 = CARTESIAN_POINT ( 'NONE',  ( 35.06754128096959988, 7.552872603316687083, -19.78349999999998943 ) ) ;
#15581 = APPROVAL_PERSON_ORGANIZATION ( #23369, #11152, #1874 ) ;
#15582 = ORIENTED_EDGE ( 'NONE', *, *, #241, .T. ) ;
#15583 = PERSON_AND_ORGANIZATION_ROLE ( 'creator' ) ;
#15584 = CARTESIAN_POINT ( 'NONE',  ( 122.4288069621910040, 9.746871424029281528, -13.00000000000000000 ) ) ;
#15585 = AXIS2_PLACEMENT_3D ( 'NONE', #47, #21549, #7322 ) ;
#15586 = APPROVAL_PERSON_ORGANIZATION ( #1991, #10397, #20169 ) ;
#15587 = DIRECTION ( 'NONE',  ( 0.9730401042858024541, -0.2306359803922080898, -5.959266323858942451E-17 ) ) ;
#15588 = COORDINATED_UNIVERSAL_TIME_OFFSET ( 0, 0, .AHEAD. ) ;
#15589 = DIRECTION ( 'NONE',  ( 0.2306359803922080343, 0.9730401042858022320, -2.572202231434325495E-16 ) ) ;
#15590 = CIRCLE ( 'NONE', #1169, 2.750000000000001332 ) ;
#15591 = ADVANCED_FACE ( 'NONE', ( #2661 ), #189, .F. ) ;
#15592 = APPROVAL ( #3643, 'UNKNOWN' ) ;
#15593 = CARTESIAN_POINT ( 'NONE',  ( -62.91457587699539289, 8.067188213978639055, 2.213507334852100055E-15 ) ) ;
#15594 = APPROVAL_DATE_TIME ( #19397, #22518 ) ;
#15595 = CC_DESIGN_APPROVAL ( #17220, ( #19768 ) ) ;
#15596 = CC_DESIGN_APPROVAL ( #9908, ( #20770 ) ) ;
#15597 = CARTESIAN_POINT ( 'NONE',  ( -29.94694237017910154, 7.343299551231789124, -2.500000000000000000 ) ) ;
#15598 = LINE ( 'NONE', #17502, #13545 ) ;
#15599 = ADVANCED_FACE ( 'NONE', ( #12803 ), #3105, .T. ) ;
#15600 = EDGE_CURVE ( 'NONE', #18635, #9514, #16578, .T. ) ;
#15601 = DIRECTION ( 'NONE',  ( -0.2306359803922026497, -0.9730401042858035643, 0.000000000000000000 ) ) ;
#15602 = DIRECTION ( 'NONE',  ( 1.000000000000000000, -2.270069654138870255E-15, -7.035747901516311190E-77 ) ) ;
#15603 = EDGE_CURVE ( 'NONE', #21456, #9901, #7562, .T. ) ;
#15604 = ORIENTED_EDGE ( 'NONE', *, *, #16593, .F. ) ;
#15605 = CC_DESIGN_APPROVAL ( #14580, ( #22797 ) ) ;
#15606 = DIRECTION ( 'NONE',  ( -0.07397971354964476276, -0.9972597464969256142, 2.428612866367529538E-15 ) ) ;
#15607 = ORIENTED_EDGE ( 'NONE', *, *, #12135, .F. ) ;
#15608 = ORIENTED_EDGE ( 'NONE', *, *, #8800, .T. ) ;
#15609 = CARTESIAN_POINT ( 'NONE',  ( 37.37362508103680625, 25.08661566644150298, -13.00000000000049916 ) ) ;
#15610 = DIRECTION ( 'NONE',  ( -0.2306359803922080898, -0.9730401042858024541, 2.572202231434325988E-16 ) ) ;
#15611 = EDGE_LOOP ( 'NONE', ( #9758, #9192, #8213, #4927 ) ) ;
#15612 = CARTESIAN_POINT ( 'NONE',  ( -60.04781580374580585, 11.89276268270289982, -5.000000000000000000 ) ) ;
#15613 = ORIENTED_EDGE ( 'NONE', *, *, #8545, .T. ) ;
#15614 = CC_DESIGN_APPROVAL ( #14012, ( #9559 ) ) ;
#15615 = CYLINDRICAL_SURFACE ( 'NONE', #12527, 0.3999999999999982458 ) ;
#15616 = DATE_TIME_ROLE ( 'classification_date' ) ;
#15617 = VECTOR ( 'NONE', #8075, 999.9999999999998863 ) ;
#15618 = DIRECTION ( 'NONE',  ( -0.9730401042858036753, 0.2306359803922031493, 5.432877459303543355E-17 ) ) ;
#15619 = EDGE_CURVE ( 'NONE', #21144, #23060, #14693, .T. ) ;
#15620 = APPROVAL_STATUS ( 'not_yet_approved' ) ;
#15621 = APPROVAL_PERSON_ORGANIZATION ( #6615, #2380, #10183 ) ;
#15622 = CYLINDRICAL_SURFACE ( 'NONE', #6573, 7.000000000000000000 ) ;
#15623 = APPROVAL ( #1301, 'UNSPECIFIED' ) ;
#15624 = CARTESIAN_POINT ( 'NONE',  ( -24.86147400983239919, -14.96352599016710094, 2.500000000000000000 ) ) ;
#15625 = DIRECTION ( 'NONE',  ( 0.000000000000000000, 0.000000000000000000, 1.000000000000000000 ) ) ;
#15626 = PRODUCT_RELATED_PRODUCT_CATEGORY ( 'detail', '', ( #12523 ) ) ;
#15627 = LINE ( 'NONE', #23211, #10781 ) ;
#15628 = EDGE_LOOP ( 'NONE', ( #14538, #11809 ) ) ;
#15629 = DIRECTION ( 'NONE',  ( -4.536707686694059956E-14, 1.228149275973191858E-30, -1.000000000000000000 ) ) ;
#15630 = EDGE_CURVE ( 'NONE', #7364, #22529, #13351, .T. ) ;
#15631 = EDGE_CURVE ( 'NONE', #1307, #16276, #13589, .T. ) ;
#15632 = DESIGN_CONTEXT ( 'detailed design', #22467, 'design' ) ;
#15633 = SECURITY_CLASSIFICATION ( '', '', #14387 ) ;
#15634 = CARTESIAN_POINT ( 'NONE',  ( -14.98746859792100139, 26.70208920133150343, -5.499999999996710187 ) ) ;
#15635 = VERTEX_POINT ( 'NONE', #79 ) ;
#15636 = CARTESIAN_POINT ( 'NONE',  ( 34.99900037908246020, 11.75885530842037241, -8.819862741542964457 ) ) ;
#15637 = DIRECTION ( 'NONE',  ( 0.9730401042858024541, -0.2306359803922080898, -5.959266323858942451E-17 ) ) ;
#15638 = AXIS2_PLACEMENT_3D ( 'NONE', #84, #18514, #16359 ) ;
#15639 = SECURITY_CLASSIFICATION_LEVEL ( 'unclassified' ) ;
#15640 = VECTOR ( 'NONE', #4015, 1000.000000000000000 ) ;
#15641 = DIRECTION ( 'NONE',  ( -0.2306359803922081175, -0.9730401042858022320, 1.412237191019896138E-17 ) ) ;
#15642 = EDGE_LOOP ( 'NONE', ( #15375, #8376, #17225, #17584 ) ) ;
#15643 = ORGANIZATION ( 'NAUO-ORG37', 'UNSPECIFIED', 'UNSPECIFIED' ) ;
#15644 = VERTEX_POINT ( 'NONE', #18270 ) ;
#15645 = APPROVAL_DATE_TIME ( #8170, #15029 ) ;
#15646 = AXIS2_PLACEMENT_3D ( 'NONE', #4184, #11459, #15106 ) ;
#15647 = DIRECTION ( 'NONE',  ( 2.270069654138870255E-15, 1.000000000000000000, 7.035747901516317327E-77 ) ) ;
#15648 = ORIENTED_EDGE ( 'NONE', *, *, #13580, .F. ) ;
#15649 = DIRECTION ( 'NONE',  ( -2.977235988022386522E-185, 9.605990953944227443E-124, 1.000000000000000000 ) ) ;
#15650 = PERSON_AND_ORGANIZATION ( #11966, #8758 ) ;
#15651 = EDGE_CURVE ( 'NONE', #886, #3254, #5660, .T. ) ;
#15652 = PRODUCT_DEFINITION_FORMATION_WITH_SPECIFIED_SOURCE ( 'ANY', '', #13292, .NOT_KNOWN. ) ;
#15653 = COORDINATED_UNIVERSAL_TIME_OFFSET ( 0, 0, .AHEAD. ) ;
#15654 = LINE ( 'NONE', #3061, #8924 ) ;
#15655 = VECTOR ( 'NONE', #495, 1000.000000000000000 ) ;
#15656 = CIRCLE ( 'NONE', #11116, 4.099999999999999645 ) ;
#15657 = EDGE_CURVE ( 'NONE', #11840, #8752, #12969, .T. ) ;
#15658 = VECTOR ( 'NONE', #14191, 1000.000000000000000 ) ;
#15659 = CARTESIAN_POINT ( 'NONE',  ( 117.1933702072879981, -12.34113894325840022, 18.89999999999999858 ) ) ;
#15660 = ORIENTED_EDGE ( 'NONE', *, *, #1412, .F. ) ;
#15661 = EDGE_CURVE ( 'NONE', #15073, #21187, #8441, .T. ) ;
#15662 = CIRCLE ( 'NONE', #5420, 2.500000000000000444 ) ;
#15663 = ADVANCED_FACE ( 'NONE', ( #3760 ), #877, .T. ) ;
#15664 = ORIENTED_EDGE ( 'NONE', *, *, #4777, .F. ) ;
#15665 = CIRCLE ( 'NONE', #15287, 2.499999999999998668 ) ;
#15666 = FACE_OUTER_BOUND ( 'NONE', #4754, .T. ) ;
#15667 = CARTESIAN_POINT ( 'NONE',  ( -20.00000000000000000, -20.00000000000000000, 5.000000000000000000 ) ) ;
#15668 = ORIENTED_EDGE ( 'NONE', *, *, #3312, .F. ) ;
#15669 = VECTOR ( 'NONE', #447, 1000.000000000000114 ) ;
#15670 = CC_DESIGN_APPROVAL ( #12300, ( #14124 ) ) ;
#15671 = FACE_OUTER_BOUND ( 'NONE', #17581, .T. ) ;
#15672 = FACE_OUTER_BOUND ( 'NONE', #12896, .T. ) ;
#15673 = PLANE ( 'NONE',  #18321 ) ;
#15674 = ORIENTED_EDGE ( 'NONE', *, *, #1239, .T. ) ;
#15675 = VERTEX_POINT ( 'NONE', #5908 ) ;
#15676 = DIRECTION ( 'NONE',  ( -0.9730401042858026761, 0.2306359803922063967, 0.000000000000000000 ) ) ;
#15677 = AXIS2_PLACEMENT_3D ( 'NONE', #11555, #5828, #5934 ) ;
#15678 = ORIENTED_EDGE ( 'NONE', *, *, #3000, .T. ) ;
#15679 = CIRCLE ( 'NONE', #21730, 2.066999999999999726 ) ;
#15680 = PERSON_AND_ORGANIZATION_ROLE ( 'creator' ) ;
#15681 = ORIENTED_EDGE ( 'NONE', *, *, #783, .T. ) ;
#15682 = VECTOR ( 'NONE', #3801, 1000.000000000000000 ) ;
#15683 = ORIENTED_EDGE ( 'NONE', *, *, #15951, .F. ) ;
#15684 = CARTESIAN_POINT ( 'NONE',  ( 3.061616997868384620E-16, -2.500000000000001776, 5.000000000000000000 ) ) ;
#15685 = APPROVAL_STATUS ( 'not_yet_approved' ) ;
#15686 = DIRECTION ( 'NONE',  ( 1.000000000000000000, 3.099353312215988811E-62, 0.000000000000000000 ) ) ;
#15687 = CIRCLE ( 'NONE', #18739, 5.000000000000000888 ) ;
#15688 = PRODUCT_RELATED_PRODUCT_CATEGORY ( 'detail', '', ( #23309 ) ) ;
#15689 = CC_DESIGN_SECURITY_CLASSIFICATION ( #22886, ( #23479 ) ) ;
#15690 = AXIS2_PLACEMENT_3D ( 'NONE', #2094, #14577, #20033 ) ;
#15691 =( REPRESENTATION_RELATIONSHIP ('NONE','NONE', #18121, #1107 ) REPRESENTATION_RELATIONSHIP_WITH_TRANSFORMATION ( #10941 )SHAPE_REPRESENTATION_RELATIONSHIP( ) );
#15692 = CARTESIAN_POINT ( 'NONE',  ( 117.1241794131700118, -12.63305097454420078, 15.50000000000000000 ) ) ;
#15693 = VECTOR ( 'NONE', #6109, 1000.000000000000000 ) ;
#15694 = DIRECTION ( 'NONE',  ( -1.000000000000000000, 0.000000000000000000, 0.000000000000000000 ) ) ;
#15695 = DATE_AND_TIME ( #952, #19738 ) ;
#15696 = ORIENTED_EDGE ( 'NONE', *, *, #1354, .T. ) ;
#15697 = FACE_OUTER_BOUND ( 'NONE', #9019, .T. ) ;
#15698 = CARTESIAN_POINT ( 'NONE',  ( -26.26776695296636888, -30.47499999999999787, -20.76776695296636888 ) ) ;
#15699 = ORIENTED_EDGE ( 'NONE', *, *, #11551, .F. ) ;
#15700 = CARTESIAN_POINT ( 'NONE',  ( -22.50000000397459843, 22.95208917591821773, -7.999999999995002220 ) ) ;
#15701 = FACE_BOUND ( 'NONE', #22907, .T. ) ;
#15702 = DIRECTION ( 'NONE',  ( -0.8511275218278966381, -0.5249589903860140128, 5.212440122911323074E-17 ) ) ;
#15703 = VERTEX_POINT ( 'NONE', #7690 ) ;
#15704 = DIRECTION ( 'NONE',  ( 0.005235963827117092427, -0.9999862922474493931, -2.636227439667000721E-16 ) ) ;
#15705 = COORDINATED_UNIVERSAL_TIME_OFFSET ( 0, 0, .AHEAD. ) ;
#15706 = EDGE_CURVE ( 'NONE', #19560, #2719, #11170, .T. ) ;
#15707 = VECTOR ( 'NONE', #12879, 1000.000000000000114 ) ;
#15708 = VERTEX_POINT ( 'NONE', #18390 ) ;
#15709 = ORIENTED_EDGE ( 'NONE', *, *, #16881, .F. ) ;
#15710 = CARTESIAN_POINT ( 'NONE',  ( -29.02403449025189985, 6.348118223725100151, 4.767474059747810244 ) ) ;
#15711 = DIRECTION ( 'NONE',  ( -0.2306359803922041485, -0.9730401042858032312, 4.373252460445728664E-15 ) ) ;
#15712 = FACE_OUTER_BOUND ( 'NONE', #4217, .T. ) ;
#15713 = CIRCLE ( 'NONE', #16438, 3.499999999999998224 ) ;
#15714 = CALENDAR_DATE ( 2026, 31, 10 ) ;
#15715 = DIRECTION ( 'NONE',  ( 6.123237831918399306E-17, -1.586917373610080078E-30, -1.000000000000000000 ) ) ;
#15716 = CARTESIAN_POINT ( 'NONE',  ( 36.10037903421270755, -9.768828191507939351, 3.399999999999999911 ) ) ;
#15717 = CARTESIAN_POINT ( 'NONE',  ( 113.9239269372040013, -8.791386740117969723, 3.438967838479089450E-14 ) ) ;
#15718 = SHAPE_REPRESENTATION_RELATIONSHIP ( 'NONE' , 'NONE' ,  #5493, #2553 ) ;
#15719 = DIRECTION ( 'NONE',  ( 0.2306359803922101437, 0.9730401042858017879, -4.006172263299087069E-15 ) ) ;
#15720 = PERSON_AND_ORGANIZATION_ROLE ( 'design_supplier' ) ;
#15721 = FACE_OUTER_BOUND ( 'NONE', #2468, .T. ) ;
#15722 = LINE ( 'NONE', #4792, #3301 ) ;
#15723 = PLANE ( 'NONE',  #12403 ) ;
#15724 = LINE ( 'NONE', #22953, #10919 ) ;
#15725 = FACE_OUTER_BOUND ( 'NONE', #7005, .T. ) ;
#15726 = ORIENTED_EDGE ( 'NONE', *, *, #23404, .F. ) ;
#15727 = CYLINDRICAL_SURFACE ( 'NONE', #6947, 5.000000000000000000 ) ;
#15728 = ORIENTED_EDGE ( 'NONE', *, *, #19416, .T. ) ;
#15729 = ADVANCED_FACE ( 'NONE', ( #13049 ), #11035, .T. ) ;
#15730 = PRODUCT ( 'Arm', 'Arm', '', ( #3456 ) ) ;
#15731 = ORIENTED_EDGE ( 'NONE', *, *, #14014, .T. ) ;
#15732 = DIRECTION ( 'NONE',  ( 1.213490492418610097E-15, 4.861311874477940294E-15, 1.000000000000000000 ) ) ;
#15733 = DIRECTION ( 'NONE',  ( -0.9730401042858023430, 0.2306359803922080620, 5.959266323858944916E-17 ) ) ;
#15734 = ORIENTED_EDGE ( 'NONE', *, *, #17029, .T. ) ;
#15735 = CC_DESIGN_PERSON_AND_ORGANIZATION_ASSIGNMENT ( #15759, #3280, ( #4974 ) ) ;
#15736 = PLANE ( 'NONE',  #468 ) ;
#15737 = ORIENTED_EDGE ( 'NONE', *, *, #4168, .F. ) ;
#15738 = DIRECTION ( 'NONE',  ( -0.9730401042858024541, 0.2306359803922080898, 5.959266323858723049E-17 ) ) ;
#15739 = APPROVAL_STATUS ( 'not_yet_approved' ) ;
#15740 = CARTESIAN_POINT ( 'NONE',  ( 35.09747506357100377, 11.43410645592840069, -29.25000000000050093 ) ) ;
#15741 = ADVANCED_FACE ( 'NONE', ( #11276 ), #18508, .F. ) ;
#15742 = ADVANCED_FACE ( 'NONE', ( #14584, #20394, #15368 ), #4121, .T. ) ;
#15743 = VECTOR ( 'NONE', #19967, 1000.000000000000000 ) ;
#15744 = COORDINATED_UNIVERSAL_TIME_OFFSET ( 0, 0, .AHEAD. ) ;
#15745 = CARTESIAN_POINT ( 'NONE',  ( 58.49563186522070168, 17.70675969991889787, 15.25461999999999918 ) ) ;
#15746 = EDGE_CURVE ( 'NONE', #645, #4600, #7666, .T. ) ;
#15747 = DIRECTION ( 'NONE',  ( 1.000000000000000000, 9.250447630115842075E-11, -1.144917494144692525E-14 ) ) ;
#15748 =( NAMED_UNIT ( * ) SI_UNIT ( $, .STERADIAN. ) SOLID_ANGLE_UNIT ( ) );
#15749 = LINE ( 'NONE', #1359, #6996 ) ;
#15750 = EDGE_LOOP ( 'NONE', ( #17326, #915, #22081, #6383, #5794, #19730, #2731, #2384, #18499, #20426, #18856, #15178, #19613, #21268, #15876, #21366, #5587, #6991, #1896, #14034, #8846, #2267, #7692, #5183, #20074, #22142, #20987, #13858, #15195, #21114, #21068, #22888, #19672, #6133, #7617, #1885, #8298, #883, #4664, #20325, #20306, #11139, #5614, #17980, #16730, #21224, #689, #17780 ) ) ;
#15751 = DIRECTION ( 'NONE',  ( 0.000000000000000000, -1.000000000000000000, -1.734723475976808278E-15 ) ) ;
#15752 = AXIS2_PLACEMENT_3D ( 'NONE', #6809, #19945, #19394 ) ;
#15753 = CARTESIAN_POINT ( 'NONE',  ( -14.00000000202540029, 1.899127378930379972, 8.000000000004439116 ) ) ;
#15754 = ORIENTED_EDGE ( 'NONE', *, *, #10098, .T. ) ;
#15755 = CARTESIAN_POINT ( 'NONE',  ( 33.84066803019035063, 10.87741165379667585, -8.976009386856679484 ) ) ;
#15756 = DIRECTION ( 'NONE',  ( -0.02168293104353429326, 0.9997648976141146893, -5.786235142515748320E-35 ) ) ;
#15757 = VERTEX_POINT ( 'NONE', #4798 ) ;
#15758 = EDGE_CURVE ( 'NONE', #6828, #7459, #12067, .T. ) ;
#15759 = PERSON_AND_ORGANIZATION ( #20415, #10692 ) ;
#15760 = CARTESIAN_POINT ( 'NONE',  ( -56.96862724498259922, -24.85214435119530307, -5.538187069399500051E-15 ) ) ;
#15761 = ORIENTED_EDGE ( 'NONE', *, *, #8985, .F. ) ;
#15762 = ORIENTED_EDGE ( 'NONE', *, *, #11213, .T. ) ;
#15764 = CALENDAR_DATE ( 2026, 31, 10 ) ;
#15763 = APPROVAL ( #4465, 'UNSPECIFIED' ) ;
#15765 = DIRECTION ( 'NONE',  ( -1.466984912809907930E-16, -2.805478249466190329E-20, -1.000000000000000000 ) ) ;
#15766 = ORIENTED_EDGE ( 'NONE', *, *, #10118, .T. ) ;
#15767 = APPROVAL ( #3284, 'UNSPECIFIED' ) ;
#15768 = LINE ( 'NONE', #4164, #15092 ) ;
#15769 = APPROVAL_STATUS ( 'not_yet_approved' ) ;
#15770 = EDGE_CURVE ( 'NONE', #15219, #12644, #8045, .T. ) ;
#15771 = EDGE_CURVE ( 'NONE', #3638, #12832, #6711, .T. ) ;
#15772 = CIRCLE ( 'NONE', #953, 7.000000000000000888 ) ;
#15773 = APPROVAL ( #13180, 'UNSPECIFIED' ) ;
#15774 = CONTEXT_DEPENDENT_SHAPE_REPRESENTATION ( #6752, #22185 ) ;
#15775 = CYLINDRICAL_SURFACE ( 'NONE', #7420, 2.499999999999998668 ) ;
#15776 = DIRECTION ( 'NONE',  ( -0.9730401042858022320, 0.2306359803922080343, 5.959266323858941219E-17 ) ) ;
#15777 = ORIENTED_EDGE ( 'NONE', *, *, #16282, .F. ) ;
#15778 = VERTEX_POINT ( 'NONE', #2902 ) ;
#15779 = DIRECTION ( 'NONE',  ( 0.2306359803922080343, 0.9730401042858022320, -2.572202231434325495E-16 ) ) ;
#15780 = FACE_BOUND ( 'NONE', #11177, .T. ) ;
#15781 = ORIENTED_EDGE ( 'NONE', *, *, #11639, .F. ) ;
#15782 = ADVANCED_FACE ( 'NONE', ( #10055 ), #13740, .F. ) ;
#15783 = CARTESIAN_POINT ( 'NONE',  ( -20.00000002062630244, 25.45208919256899804, 8.000000000004455103 ) ) ;
#15784 =( GEOMETRIC_REPRESENTATION_CONTEXT ( 3 ) GLOBAL_UNCERTAINTY_ASSIGNED_CONTEXT ( ( #12753 ) ) GLOBAL_UNIT_ASSIGNED_CONTEXT ( ( #19172, #1090, #6585 ) ) REPRESENTATION_CONTEXT ( 'NONE', 'WORKASPACE' ) );
#15785 = DIRECTION ( 'NONE',  ( -3.210834492181040124E-17, 2.441916418604790135E-15, 1.000000000000000000 ) ) ;
#15786 = FACE_BOUND ( 'NONE', #5910, .T. ) ;
#15787 = VERTEX_POINT ( 'NONE', #12181 ) ;
#15788 = ORIENTED_EDGE ( 'NONE', *, *, #13957, .F. ) ;
#15789 = CARTESIAN_POINT ( 'NONE',  ( -23.49893655333878684, 22.87624079303554581, 4.999999999999900524 ) ) ;
#15790 = VERTEX_POINT ( 'NONE', #22841 ) ;
#15791 = COORDINATED_UNIVERSAL_TIME_OFFSET ( 0, 0, .AHEAD. ) ;
#15792 = CIRCLE ( 'NONE', #9342, 4.999999999999998224 ) ;
#15793 = VERTEX_POINT ( 'NONE', #8716 ) ;
#15794 = ORIENTED_EDGE ( 'NONE', *, *, #22919, .F. ) ;
#15795 = DIRECTION ( 'NONE',  ( -0.9730401042858022320, 0.2306359803922080343, 5.959266323858941219E-17 ) ) ;
#15796 = PERSON_AND_ORGANIZATION ( #11966, #8758 ) ;
#15797 = EDGE_CURVE ( 'NONE', #4103, #12681, #10280, .T. ) ;
#15798 = ADVANCED_FACE ( 'NONE', ( #13832 ), #21417, .F. ) ;
#15799 = DIRECTION ( 'NONE',  ( -0.9730401042858024541, 0.2306359803922080898, 5.959266323858942451E-17 ) ) ;
#15800 = CIRCLE ( 'NONE', #7461, 3.999999999999998668 ) ;
#15801 = VECTOR ( 'NONE', #23417, 1000.000000000000000 ) ;
#15802 = DIRECTION ( 'NONE',  ( -0.2306359803922028995, -0.9730401042858036753, 4.730251413307818851E-15 ) ) ;
#15803 = SECURITY_CLASSIFICATION_LEVEL ( 'unclassified' ) ;
#15804 = EDGE_LOOP ( 'NONE', ( #18247, #14081, #750, #7785 ) ) ;
#15805 = DIRECTION ( 'NONE',  ( 8.410780489584519664E-16, -1.000000000000000000, 0.000000000000000000 ) ) ;
#15806 = DIRECTION ( 'NONE',  ( 0.02167246311338769799, -0.9997651245880698756, 2.441989331389200018E-15 ) ) ;
#15807 = ORIENTED_EDGE ( 'NONE', *, *, #2230, .F. ) ;
#15808 = EDGE_CURVE ( 'NONE', #4850, #4506, #17508, .T. ) ;
#15809 = CARTESIAN_POINT ( 'NONE',  ( -27.00000000000000000, -20.00000000000000000, 5.000000000000000000 ) ) ;
#15810 = CARTESIAN_POINT ( 'NONE',  ( 38.19845176233020823, -1.855887187839940777, 13.00000000000000000 ) ) ;
#15811 = DIRECTION ( 'NONE',  ( -0.9730401042858038974, 0.2306359803922014562, -1.121193430162461718E-15 ) ) ;
#15812 = VERTEX_POINT ( 'NONE', #19180 ) ;
#15813 = LINE ( 'NONE', #2762, #12628 ) ;
#15814 = CALENDAR_DATE ( 2026, 31, 10 ) ;
#15815 = CIRCLE ( 'NONE', #13159, 3.499999999999999556 ) ;
#15816 = VERTEX_POINT ( 'NONE', #11957 ) ;
#15817 = ORIENTED_EDGE ( 'NONE', *, *, #18926, .F. ) ;
#15818 = DIRECTION ( 'NONE',  ( -1.187319687680494078E-16, -2.805478249478260493E-20, -1.000000000000000000 ) ) ;
#15819 = AXIS2_PLACEMENT_3D ( 'NONE', #15667, #21467, #6767 ) ;
#15820 = CARTESIAN_POINT ( 'NONE',  ( -67.26895854462263458, 12.68829727884599201, 2.499999999999999556 ) ) ;
#15821 = CIRCLE ( 'NONE', #2918, 2.499999999999999556 ) ;
#15822 = CARTESIAN_POINT ( 'NONE',  ( -65.64475015647069256, -21.84411297095480009, 5.000000000000000000 ) ) ;
#15823 = COORDINATED_UNIVERSAL_TIME_OFFSET ( 0, 0, .AHEAD. ) ;
#15824 = EDGE_CURVE ( 'NONE', #8556, #19315, #3246, .T. ) ;
#15825 = FACE_OUTER_BOUND ( 'NONE', #3279, .T. ) ;
#15826 = CARTESIAN_POINT ( 'NONE',  ( -20.00000000397400157, 22.95208919257349933, -5.499999999995569766 ) ) ;
#15827 = CARTESIAN_POINT ( 'NONE',  ( -20.00000000000000000, -25.00000000000000000, -4.999999999995459632 ) ) ;
#15828 =( BOUNDED_CURVE ( )  B_SPLINE_CURVE ( 2, ( #3657, #18275, #9358 ),
 .UNSPECIFIED., .F., .F. ) 
 B_SPLINE_CURVE_WITH_KNOTS ( ( 3, 3 ),
 ( 0.000000000000000000, 0.2336872276155859962 ),
 .UNSPECIFIED. ) 
 CURVE ( )  GEOMETRIC_REPRESENTATION_ITEM ( )  RATIONAL_B_SPLINE_CURVE ( ( 1.000000000000000000, 1.154700538379249908, 1.000000000000000000 ) ) 
 REPRESENTATION_ITEM ( '' )  );
#15829 =( NAMED_UNIT ( * ) SI_UNIT ( $, .STERADIAN. ) SOLID_ANGLE_UNIT ( ) );
#15830 = AXIS2_PLACEMENT_3D ( 'NONE', #14865, #6315, #5961 ) ;
#15831 = VERTEX_POINT ( 'NONE', #11829 ) ;
#15832 = FACE_OUTER_BOUND ( 'NONE', #2827, .T. ) ;
#15833 = CALENDAR_DATE ( 2026, 31, 10 ) ;
#15834 = VECTOR ( 'NONE', #23199, 1000.000000000000000 ) ;
#15835 = TOROIDAL_SURFACE ( 'NONE', #19245, 2.600000000000000089, 0.1000000000000000056 ) ;
#15836 = CARTESIAN_POINT ( 'NONE',  ( 36.90976272218952658, 8.157610693807670899, 8.912036319352676372 ) ) ;
#15837 = DIRECTION ( 'NONE',  ( -1.466984912809907930E-16, -2.805478249466190329E-20, -1.000000000000000000 ) ) ;
#15838 = CARTESIAN_POINT ( 'NONE',  ( 1.406882533891259834, 17.87809865158410005, -7.060250502199809043E-15 ) ) ;
#15839 = FACE_OUTER_BOUND ( 'NONE', #4001, .T. ) ;
#15840 = CARTESIAN_POINT ( 'NONE',  ( 5.000000000000000000, -28.60000000000000142, -2.500000000000000000 ) ) ;
#15841 = ORIENTED_EDGE ( 'NONE', *, *, #18634, .T. ) ;
#15842 = CARTESIAN_POINT ( 'NONE',  ( 34.87444594764019712, 25.38231313435129977, 12.50000000000000000 ) ) ;
#15843 = UNCERTAINTY_MEASURE_WITH_UNIT (LENGTH_MEASURE( 1.000000000000000082E-05 ), #14771, 'distance_accuracy_value', 'NONE');
#15844 = ORIENTED_EDGE ( 'NONE', *, *, #20920, .T. ) ;
#15845 = DIRECTION ( 'NONE',  ( -1.159535895544890222E-14, -2.167612681253619929E-15, -1.000000000000000000 ) ) ;
#15846 = CARTESIAN_POINT ( 'NONE',  ( 27.94580623989299895, -3.849224340072180173, -12.50000000000040146 ) ) ;
#15847 = AXIS2_PLACEMENT_3D ( 'NONE', #4770, #12035, #17471 ) ;
#15848 = ORIENTED_EDGE ( 'NONE', *, *, #18087, .T. ) ;
#15849 = DIRECTION ( 'NONE',  ( -0.9730401042858022320, 0.2306359803922080343, 5.959266323858941219E-17 ) ) ;
#15850 = AXIS2_PLACEMENT_3D ( 'NONE', #5404, #9321, #3731 ) ;
#15851 = ORIENTED_EDGE ( 'NONE', *, *, #14015, .F. ) ;
#15852 = FACE_OUTER_BOUND ( 'NONE', #22569, .T. ) ;
#15853 = DATE_AND_TIME ( #19304, #10761 ) ;
#15854 = CARTESIAN_POINT ( 'NONE',  ( 36.09092202081949807, 8.115512906978459284, 27.68999999999999773 ) ) ;
#15855 = APPROVAL_DATE_TIME ( #19307, #6606 ) ;
#15856 = DIRECTION ( 'NONE',  ( -0.6944962871189153120, 0.7194962871190101472, 0.000000000000000000 ) ) ;
#15857 = EDGE_CURVE ( 'NONE', #16294, #14214, #19064, .T. ) ;
#15858 = DIRECTION ( 'NONE',  ( -0.9997648975362233292, -0.02168293463497958373, 0.000000000000000000 ) ) ;
#15859 = AXIS2_PLACEMENT_3D ( 'NONE', #11309, #2242, #22191 ) ;
#15860 = LINE ( 'NONE', #19544, #16453 ) ;
#15861 = ORIENTED_EDGE ( 'NONE', *, *, #17910, .F. ) ;
#15862 = CARTESIAN_POINT ( 'NONE',  ( -30.79248430819469817, 6.338858557518999959, 3.000000000000090150 ) ) ;
#15863 = PLANE ( 'NONE',  #9928 ) ;
#15864 = VECTOR ( 'NONE', #3943, 1000.000000000000227 ) ;
#15865 = VERTEX_POINT ( 'NONE', #3135 ) ;
#15866 = CARTESIAN_POINT ( 'NONE',  ( 36.07092311366587722, 11.78608357701199694, -37.44562646538080486 ) ) ;
#15867 = CARTESIAN_POINT ( 'NONE',  ( -20.00000000397270128, 22.95208919256889857, -5.448922613368719782E-15 ) ) ;
#15868 = ADVANCED_FACE ( 'NONE', ( #21297 ), #23183, .F. ) ;
#15869 = EDGE_LOOP ( 'NONE', ( #4861, #7819, #5324, #3103 ) ) ;
#15870 = DATE_TIME_ROLE ( 'classification_date' ) ;
#15871 = DIRECTION ( 'NONE',  ( -4.040376328279780192E-15, 1.000000000000000000, 0.000000000000000000 ) ) ;
#15872 = VERTEX_POINT ( 'NONE', #13942 ) ;
#15873 = EDGE_LOOP ( 'NONE', ( #19807, #5997 ) ) ;
#15874 = CALENDAR_DATE ( 2026, 31, 10 ) ;
#15875 = FACE_OUTER_BOUND ( 'NONE', #21683, .T. ) ;
#15876 = ORIENTED_EDGE ( 'NONE', *, *, #10661, .F. ) ;
#15877 = CARTESIAN_POINT ( 'NONE',  ( 39.74442752440959481, 5.605205456207790427, -19.59999999999999787 ) ) ;
#15878 = APPROVAL_DATE_TIME ( #3291, #23437 ) ;
#15879 = DATE_AND_TIME ( #3186, #10696 ) ;
#15880 = AXIS2_PLACEMENT_3D ( 'NONE', #17248, #17114, #6308 ) ;
#15881 = PLANE ( 'NONE',  #11612 ) ;
#15882 = ADVANCED_FACE ( 'NONE', ( #15725 ), #10408, .T. ) ;
#15883 = DIRECTION ( 'NONE',  ( 0.000000000000000000, 1.000000000000000000, 0.000000000000000000 ) ) ;
#15884 = EDGE_LOOP ( 'NONE', ( #4654, #20953, #6212, #20445 ) ) ;
#15885 = CC_DESIGN_PERSON_AND_ORGANIZATION_ASSIGNMENT ( #9849, #18773, ( #10620 ) ) ;
#15886 = APPROVAL ( #11210, 'UNSPECIFIED' ) ;
#15887 = EDGE_LOOP ( 'NONE', ( #10572, #16725, #7969, #12801 ) ) ;
#15888 = LINE ( 'NONE', #14348, #8419 ) ;
#15889 = FACE_OUTER_BOUND ( 'NONE', #17101, .T. ) ;
#15890 = EDGE_LOOP ( 'NONE', ( #2374, #4361, #14215, #12838, #3469, #23184, #1614, #21991, #20958, #3071, #13672, #21772 ) ) ;
#15891 = ADVANCED_FACE ( 'NONE', ( #8605, #17397 ), #15952, .T. ) ;
#15892 = ADVANCED_FACE ( 'NONE', ( #22713 ), #6458, .F. ) ;
#15893 = DIRECTION ( 'NONE',  ( 0.9999862922474493931, 0.005235963827108368503, 0.000000000000000000 ) ) ;
#15894 = DIRECTION ( 'NONE',  ( -4.539762594625140272E-47, -1.000000000000000000, 0.000000000000000000 ) ) ;
#15895 = ORIENTED_EDGE ( 'NONE', *, *, #16465, .T. ) ;
#15896 = ORIENTED_EDGE ( 'NONE', *, *, #8656, .T. ) ;
#15897 = LINE ( 'NONE', #285, #13620 ) ;
#15898 = ORIENTED_EDGE ( 'NONE', *, *, #6373, .F. ) ;
#15899 = PERSON_AND_ORGANIZATION ( #11966, #8758 ) ;
#15900 = EDGE_CURVE ( 'NONE', #1899, #2844, #8952, .T. ) ;
#15901 = EDGE_LOOP ( 'NONE', ( #7439, #297, #20617, #19137 ) ) ;
#15902 = ORIENTED_EDGE ( 'NONE', *, *, #8140, .T. ) ;
#15903 = CARTESIAN_POINT ( 'NONE',  ( 33.90884364377009774, 10.17428291754630010, 29.25000000000000000 ) ) ;
#15904 = CARTESIAN_POINT ( 'NONE',  ( -20.00000000397080058, 22.95208919256900160, 8.500000000004460432 ) ) ;
#15905 = APPROVAL_ROLE ( '' ) ;
#15906 = VECTOR ( 'NONE', #6325, 1000.000000000000000 ) ;
#15907 = CARTESIAN_POINT ( 'NONE',  ( -0.9605240398339689456, 18.43923599187829865, -8.566766326431390468E-17 ) ) ;
#15908 = EDGE_CURVE ( 'NONE', #17960, #22329, #19881, .T. ) ;
#15909 = DIRECTION ( 'NONE',  ( 6.124378941434239724E-17, -2.274246353359159970E-33, 1.000000000000000000 ) ) ;
#15910 = CC_DESIGN_DATE_AND_TIME_ASSIGNMENT ( #16021, #19589, ( #8452 ) ) ;
#15911 = COORDINATED_UNIVERSAL_TIME_OFFSET ( 0, 0, .AHEAD. ) ;
#15912 = PRODUCT ( '1602p_c_42', '1602p_c_42', '', ( #1419 ) ) ;
#15913 = CC_DESIGN_DATE_AND_TIME_ASSIGNMENT ( #2499, #16613, ( #13468 ) ) ;
#15914 = ORIENTED_EDGE ( 'NONE', *, *, #15603, .T. ) ;
#15915 = CARTESIAN_POINT ( 'NONE',  ( -25.01253141238839817, 26.70208918381559826, -7.999999999994430233 ) ) ;
#15916 = CARTESIAN_POINT ( 'NONE',  ( -20.00000000000000000, -20.00000000000000000, -4.999999999995470290 ) ) ;
#15917 = ORIENTED_EDGE ( 'NONE', *, *, #2083, .F. ) ;
#15918 = EDGE_CURVE ( 'NONE', #15708, #14674, #2357, .T. ) ;
#15919 = EDGE_CURVE ( 'NONE', #14674, #15703, #11096, .T. ) ;
#15920 = LINE ( 'NONE', #3101, #7130 ) ;
#15921 = LINE ( 'NONE', #7036, #5462 ) ;
#15922 = CYLINDRICAL_SURFACE ( 'NONE', #13369, 2.500000000000000888 ) ;
#15923 = ORIENTED_EDGE ( 'NONE', *, *, #352, .F. ) ;
#15924 = TOROIDAL_SURFACE ( 'NONE', #5677, 2.380000000000000338, 2.370000000000000107 ) ;
#15925 = CARTESIAN_POINT ( 'NONE',  ( 52.73786095581300515, -7.648876468381139659, 15.00924000000014935 ) ) ;
#15926 = APPROVAL_STATUS ( 'not_yet_approved' ) ;
#15927 = VERTEX_POINT ( 'NONE', #12643 ) ;
#15928 = ORIENTED_EDGE ( 'NONE', *, *, #5299, .F. ) ;
#15929 = DIRECTION ( 'NONE',  ( 0.2306359803922053142, 0.9730401042858028982, 0.000000000000000000 ) ) ;
#15930 = CARTESIAN_POINT ( 'NONE',  ( 39.37089837072289811, 22.23982225285509884, 13.00000000000000000 ) ) ;
#15931 = DIRECTION ( 'NONE',  ( 0.005235963827117092427, -0.9999862922474493931, -2.636227439667000721E-16 ) ) ;
#15932 = PERSON_AND_ORGANIZATION ( #11966, #8758 ) ;
#15933 = DIRECTION ( 'NONE',  ( -0.2306359803922080343, -0.9730401042858022320, -7.611545645953073104E-14 ) ) ;
#15934 = LOCAL_TIME ( 14, 11, 27.00000000000000000, #10948 ) ;
#15935 = CARTESIAN_POINT ( 'NONE',  ( 113.2033677465029911, -29.17473274740279976, 3.100000000000039613 ) ) ;
#15936 =( GEOMETRIC_REPRESENTATION_CONTEXT ( 3 ) GLOBAL_UNCERTAINTY_ASSIGNED_CONTEXT ( ( #21985 ) ) GLOBAL_UNIT_ASSIGNED_CONTEXT ( ( #11409, #18646, #21832 ) ) REPRESENTATION_CONTEXT ( 'NONE', 'WORKASPACE' ) );
#15937 = EDGE_CURVE ( 'NONE', #17080, #13190, #5007, .T. ) ;
#15938 = DIRECTION ( 'NONE',  ( 0.000000000000000000, 0.000000000000000000, 1.000000000000000000 ) ) ;
#15939 = AXIS2_PLACEMENT_3D ( 'NONE', #13451, #20221, #9665 ) ;
#15940 = CARTESIAN_POINT ( 'NONE',  ( -16.00004797695772751, -0.08377682083104373567, 9.108728376131438406E-14 ) ) ;
#15941 = PERSON_AND_ORGANIZATION ( #11966, #8758 ) ;
#15942 = ADVANCED_FACE ( 'NONE', ( #10756 ), #11494, .F. ) ;
#15943 = VECTOR ( 'NONE', #3349, 1000.000000000000227 ) ;
#15944 = CARTESIAN_POINT ( 'NONE',  ( 36.20429989730508424, 11.75446978728179559, 8.759424124907038589 ) ) ;
#15945 = LINE ( 'NONE', #9177, #4441 ) ;
#15946 = APPLICATION_CONTEXT ( 'configuration controlled 3d designs of mechanical parts and assemblies' ) ;
#15947 = EDGE_CURVE ( 'NONE', #7459, #18433, #12233, .T. ) ;
#15948 = DIRECTION ( 'NONE',  ( -0.2306359803922054252, -0.9730401042858028982, 0.000000000000000000 ) ) ;
#15949 = LOCAL_TIME ( 14, 11, 27.00000000000000000, #22552 ) ;
#15950 = CYLINDRICAL_SURFACE ( 'NONE', #21884, 2.500000000000000000 ) ;
#15951 = EDGE_CURVE ( 'NONE', #20315, #8432, #19752, .T. ) ;
#15952 = PLANE ( 'NONE',  #23198 ) ;
#15953 = LOCAL_TIME ( 14, 11, 27.00000000000000000, #22129 ) ;
#15954 = VERTEX_POINT ( 'NONE', #7522 ) ;
#15955 = DIRECTION ( 'NONE',  ( -0.4865200521429013936, 0.1153179901961013387, -0.8660254037844388186 ) ) ;
#15956 = ORIENTED_EDGE ( 'NONE', *, *, #5261, .F. ) ;
#15957 = DIRECTION ( 'NONE',  ( -3.210834492181139964E-17, 2.441916418604790135E-15, 1.000000000000000000 ) ) ;
#15958 = CARTESIAN_POINT ( 'NONE',  ( 6.272083055320289979, 16.72491874962310021, -5.657758596979629988E-15 ) ) ;
#15959 = EDGE_LOOP ( 'NONE', ( #20500, #4709 ) ) ;
#15960 = CIRCLE ( 'NONE', #22017, 2.066999999999998394 ) ;
#15961 = CARTESIAN_POINT ( 'NONE',  ( -16.00004797695752501, -0.08377682083102050425, 2.499999999999999556 ) ) ;
#15962 = VERTEX_POINT ( 'NONE', #2051 ) ;
#15963 = LINE ( 'NONE', #5269, #18874 ) ;
#15964 = SHAPE_REPRESENTATION ( 'Nut', ( #12739 ), #2264 ) ;
#15965 = LINE ( 'NONE', #19421, #15834 ) ;
#15966 = LOCAL_TIME ( 14, 11, 27.00000000000000000, #1995 ) ;
#15967 = SHAPE_REPRESENTATION_RELATIONSHIP ( 'NONE' , 'NONE' ,  #15060, #3675 ) ;
#15968 = CC_DESIGN_APPROVAL ( #22518, ( #9917 ) ) ;
#15969 = LINE ( 'NONE', #10775, #19463 ) ;
#15970 = CC_DESIGN_PERSON_AND_ORGANIZATION_ASSIGNMENT ( #16995, #10019, ( #3051 ) ) ;
#15971 = AXIS2_PLACEMENT_3D ( 'NONE', #21927, #11277, #18509 ) ;
#15972 = CARTESIAN_POINT ( 'NONE',  ( -55.82581668011050624, -8.866088801542479914, 7.200000000000000178 ) ) ;
#15973 = APPROVAL_PERSON_ORGANIZATION ( #5651, #4717, #18382 ) ;
#15974 = DIRECTION ( 'NONE',  ( 1.138590270679734009E-14, 2.220446049251240387E-15, 1.000000000000000000 ) ) ;
#15975 = ORIENTED_EDGE ( 'NONE', *, *, #17769, .T. ) ;
#15977 = CIRCLE ( 'NONE', #19023, 3.499999999999998668 ) ;
#15976 = DIRECTION ( 'NONE',  ( -0.8511275218278966381, -0.5249589903860140128, 5.212440122911323074E-17 ) ) ;
#15978 = DIRECTION ( 'NONE',  ( 1.000000000000000000, 0.000000000000000000, 0.000000000000000000 ) ) ;
#15979 = ORIENTED_EDGE ( 'NONE', *, *, #14514, .F. ) ;
#15980 = CARTESIAN_POINT ( 'NONE',  ( 35.53353590478442214, 11.84532598660267233, -8.774845639078000303 ) ) ;
#15981 = CARTESIAN_POINT ( 'NONE',  ( -19.49999999982379961, -0.1021026942259709996, 2.500000000000090150 ) ) ;
#15982 = ORIENTED_EDGE ( 'NONE', *, *, #11617, .T. ) ;
#15983 = APPROVAL_PERSON_ORGANIZATION ( #13867, #12304, #12223 ) ;
#15984 = APPROVAL_DATE_TIME ( #8986, #23109 ) ;
#15985 = FACE_BOUND ( 'NONE', #19821, .T. ) ;
#15986 = CC_DESIGN_APPROVAL ( #4793, ( #1510 ) ) ;
#15987 = ORIENTED_EDGE ( 'NONE', *, *, #18437, .F. ) ;
#15988 = ORIENTED_EDGE ( 'NONE', *, *, #13985, .F. ) ;
#15989 = VECTOR ( 'NONE', #16724, 999.9999999999998863 ) ;
#15990 = AXIS2_PLACEMENT_3D ( 'NONE', #22939, #8588, #8703 ) ;
#15991 = APPROVAL_ROLE ( '' ) ;
#15992 = CARTESIAN_POINT ( 'NONE',  ( -20.00000000397270128, 22.95208919256889857, -2.500000000000000000 ) ) ;
#15993 = ADVANCED_FACE ( 'NONE', ( #12750 ), #141, .T. ) ;
#15994 = VERTEX_POINT ( 'NONE', #14528 ) ;
#15995 = CARTESIAN_POINT ( 'NONE',  ( -25.49858938551139786, -0.2322002804899429840, -2.500000000000000000 ) ) ;
#15996 = LOCAL_TIME ( 14, 11, 27.00000000000000000, #17044 ) ;
#15997 = PERSON_AND_ORGANIZATION ( #11966, #8758 ) ;
#15998 = APPROVAL_PERSON_ORGANIZATION ( #20208, #6025, #5591 ) ;
#15999 = DIRECTION ( 'NONE',  ( -2.270069654138870255E-15, -1.000000000000000000, -7.035747901516317327E-77 ) ) ;
#16000 = VECTOR ( 'NONE', #19290, 1000.000000000000000 ) ;
#16001 = ORIENTED_EDGE ( 'NONE', *, *, #14022, .F. ) ;
#16002 = AXIS2_PLACEMENT_3D ( 'NONE', #22531, #18871, #22288 ) ;
#16003 = AXIS2_PLACEMENT_3D ( 'NONE', #9326, #14561, #18239 ) ;
#16004 = ORIENTED_EDGE ( 'NONE', *, *, #5470, .T. ) ;
#16005 = CC_DESIGN_SECURITY_CLASSIFICATION ( #17552, ( #23504 ) ) ;
#16006 = CARTESIAN_POINT ( 'NONE',  ( 0.03739227630228923044, 20.77197087308299572, -2.849987155837237711E-16 ) ) ;
#16007 = DIRECTION ( 'NONE',  ( -2.972463603623604872E-47, -1.000000000000000000, -2.972463603623604872E-47 ) ) ;
#16008 = ORIENTED_EDGE ( 'NONE', *, *, #14312, .T. ) ;
#16009 = VECTOR ( 'NONE', #18809, 1000.000000000000227 ) ;
#16010 = AXIS2_PLACEMENT_3D ( 'NONE', #1901, #16053, #19733 ) ;
#16011 = CARTESIAN_POINT ( 'NONE',  ( -20.00000000397270128, 22.95208919256889857, 2.500000000000000000 ) ) ;
#16012 = CARTESIAN_POINT ( 'NONE',  ( 52.26033179423370001, -7.535689554643993482, -15.50000000000040146 ) ) ;
#16013 = ORIENTED_EDGE ( 'NONE', *, *, #21053, .T. ) ;
#16014 = ORIENTED_EDGE ( 'NONE', *, *, #17007, .T. ) ;
#16015 = APPROVAL_DATE_TIME ( #1869, #10557 ) ;
#16016 = ADVANCED_FACE ( 'NONE', ( #251 ), #21766, .T. ) ;
#16017 = APPROVAL_PERSON_ORGANIZATION ( #18981, #8661, #20519 ) ;
#16018 = VERTEX_POINT ( 'NONE', #18332 ) ;
#16019 = EDGE_LOOP ( 'NONE', ( #21875, #9011 ) ) ;
#16020 = LINE ( 'NONE', #12813, #2392 ) ;
#16021 = DATE_AND_TIME ( #8678, #11881 ) ;
#16022 = CIRCLE ( 'NONE', #3514, 2.500000000000000888 ) ;
#16023 = CIRCLE ( 'NONE', #20201, 2.499999999999998668 ) ;
#16024 = CC_DESIGN_PERSON_AND_ORGANIZATION_ASSIGNMENT ( #2328, #4109, ( #12599 ) ) ;
#16025 = VECTOR ( 'NONE', #17642, 1000.000000000000000 ) ;
#16026 = CARTESIAN_POINT ( 'NONE',  ( -19.49999999982379961, -0.1021026942259709996, 9.160072195675308484E-14 ) ) ;
#16027 = COORDINATED_UNIVERSAL_TIME_OFFSET ( 0, 0, .AHEAD. ) ;
#16028 = ADVANCED_FACE ( 'NONE', ( #14642 ), #1921, .F. ) ;
#16029 = EDGE_CURVE ( 'NONE', #8698, #7573, #5610, .T. ) ;
#16030 = CIRCLE ( 'NONE', #18714, 2.458500000000000352 ) ;
#16032 = AXIS2_PLACEMENT_3D ( 'NONE', #21935, #16710, #4134 ) ;
#16031 = CYLINDRICAL_SURFACE ( 'NONE', #5818, 2.458500000000000352 ) ;
#16033 = AXIS2_PLACEMENT_3D ( 'NONE', #12458, #2948, #15883 ) ;
#16034 = DATE_TIME_ROLE ( 'creation_date' ) ;
#16035 = LOCAL_TIME ( 14, 11, 27.00000000000000000, #9459 ) ;
#16036 = VERTEX_POINT ( 'NONE', #3822 ) ;
#16037 = LINE ( 'NONE', #16691, #15196 ) ;
#16038 = DIRECTION ( 'NONE',  ( -5.964507377817269296E-17, -4.861311874385510251E-15, -1.000000000000000000 ) ) ;
#16039 = ORIENTED_EDGE ( 'NONE', *, *, #3383, .T. ) ;
#16040 = CIRCLE ( 'NONE', #3147, 5.000000000000000888 ) ;
#16041 = CARTESIAN_POINT ( 'NONE',  ( 113.8430260960419957, 8.210644904773758412, 2.067000000000030369 ) ) ;
#16042 = AXIS2_PLACEMENT_3D ( 'NONE', #15114, #7879, #11702 ) ;
#16043 = CARTESIAN_POINT ( 'NONE',  ( -29.94694237017910154, 7.343299551231789124, -3.750000000000000000 ) ) ;
#16044 = CARTESIAN_POINT ( 'NONE',  ( -16.50058068176714343, 23.02794805996801841, 5.000000000000000000 ) ) ;
#16045 = VERTEX_POINT ( 'NONE', #14753 ) ;
#16046 = ORIENTED_EDGE ( 'NONE', *, *, #20324, .F. ) ;
#16047 = DIRECTION ( 'NONE',  ( 0.9730401042858036753, -0.2306359803922031493, 2.804983810440361760E-16 ) ) ;
#16048 = APPROVAL_ROLE ( '' ) ;
#16049 = EDGE_CURVE ( 'NONE', #1281, #9901, #14170, .T. ) ;
#16050 = EDGE_LOOP ( 'NONE', ( #21799, #18534, #13854, #5658 ) ) ;
#16051 = VERTEX_POINT ( 'NONE', #17858 ) ;
#16052 = CYLINDRICAL_SURFACE ( 'NONE', #8443, 4.250000000000000000 ) ;
#16053 = DIRECTION ( 'NONE',  ( -0.9730401042858024541, 0.2306359803922080898, 5.959266323858232476E-17 ) ) ;
#16054 = AXIS2_PLACEMENT_3D ( 'NONE', #10592, #17817, #12482 ) ;
#16055 = CARTESIAN_POINT ( 'NONE',  ( 6.500000000000000000, -1.630990338096509915E-14, 2.500000000000000000 ) ) ;
#16056 = CALENDAR_DATE ( 2026, 31, 10 ) ;
#16057 = CARTESIAN_POINT ( 'NONE',  ( 26.11627841292210306, -8.532812502301741375, -20.00000000000000000 ) ) ;
#16058 = CC_DESIGN_PERSON_AND_ORGANIZATION_ASSIGNMENT ( #10065, #20962, ( #17948 ) ) ;
#16059 = CC_DESIGN_APPROVAL ( #12001, ( #18743 ) ) ;
#16060 = AXIS2_PLACEMENT_3D ( 'NONE', #6979, #21322, #4938 ) ;
#16061 = CC_DESIGN_DATE_AND_TIME_ASSIGNMENT ( #10447, #10204, ( #9559 ) ) ;
#16062 = DIRECTION ( 'NONE',  ( 0.000000000000000000, -1.000000000000000000, 2.081668171172169697E-15 ) ) ;
#16063 = VECTOR ( 'NONE', #16216, 999.9999999999998863 ) ;
#16064 = ADVANCED_FACE ( 'NONE', ( #1572 ), #16077, .F. ) ;
#16065 = ADVANCED_FACE ( 'NONE', ( #21520 ), #2162, .F. ) ;
#16066 = CIRCLE ( 'NONE', #22828, 2.999765877365279998 ) ;
#16067 = CC_DESIGN_DATE_AND_TIME_ASSIGNMENT ( #10379, #8466, ( #11807 ) ) ;
#16068 = CARTESIAN_POINT ( 'NONE',  ( 0.000000000000000000, 0.000000000000000000, 0.000000000000000000 ) ) ;
#16069 = CARTESIAN_POINT ( 'NONE',  ( -4.514225866272930432, 4.676725866273559795, 5.000000000000000000 ) ) ;
#16070 = APPROVAL_DATE_TIME ( #14050, #16991 ) ;
#16071 = FACE_OUTER_BOUND ( 'NONE', #3658, .T. ) ;
#16072 = VECTOR ( 'NONE', #18311, 1000.000000000000000 ) ;
#16073 = CARTESIAN_POINT ( 'NONE',  ( 33.37436288052550282, -3.059220458576419777, -13.00000000000039968 ) ) ;
#16074 = DIRECTION ( 'NONE',  ( 0.000000000000000000, 0.000000000000000000, -1.000000000000000000 ) ) ;
#16075 = AXIS2_PLACEMENT_3D ( 'NONE', #14341, #11268, #16462 ) ;
#16076 = DIRECTION ( 'NONE',  ( -0.9730401042858035643, 0.2306359803922028717, 5.959266323858677443E-17 ) ) ;
#16077 = PLANE ( 'NONE',  #18288 ) ;
#16078 = ORIENTED_EDGE ( 'NONE', *, *, #13760, .F. ) ;
#16079 = DIRECTION ( 'NONE',  ( -0.2306359803922028162, -0.9730401042858034533, 1.407521210652564497E-17 ) ) ;
#16080 = ADVANCED_FACE ( 'NONE', ( #14985 ), #11692, .F. ) ;
#16081 = ORIENTED_EDGE ( 'NONE', *, *, #12693, .F. ) ;
#16082 = CARTESIAN_POINT ( 'NONE',  ( 38.13838090529419844, 22.53196116135175231, -13.00000000000049916 ) ) ;
#16083 = DIRECTION ( 'NONE',  ( 0.9999862922474492821, 0.005235963827109980928, 0.000000000000000000 ) ) ;
#16084 = VERTEX_POINT ( 'NONE', #22464 ) ;
#16085 = CARTESIAN_POINT ( 'NONE',  ( 31.11077410011089839, -1.335996977273150144, 11.00000000000019895 ) ) ;
#16086 = EDGE_CURVE ( 'NONE', #13198, #20578, #1258, .T. ) ;
#16087 = EDGE_LOOP ( 'NONE', ( #6533, #17751, #3794, #5096 ) ) ;
#16088 = DIRECTION ( 'NONE',  ( 0.9730401042858035643, -0.2306359803922028717, -5.959266323858667582E-17 ) ) ;
#16089 = CALENDAR_DATE ( 2026, 31, 10 ) ;
#16090 = CYLINDRICAL_SURFACE ( 'NONE', #4828, 8.000000000000003553 ) ;
#16091 = EDGE_CURVE ( 'NONE', #20507, #10293, #5722, .T. ) ;
#16092 = CIRCLE ( 'NONE', #12322, 2.499999999999998668 ) ;
#16093 = EDGE_CURVE ( 'NONE', #21263, #12681, #17163, .T. ) ;
#16094 = AXIS2_PLACEMENT_3D ( 'NONE', #23361, #8663, #15893 ) ;
#16095 = DIRECTION ( 'NONE',  ( 0.2306359803922080620, 0.9730401042858023430, 1.268685090138121373E-13 ) ) ;
#16096 = CARTESIAN_POINT ( 'NONE',  ( 36.78282996199610722, 11.03463321983559986, -27.69000000000049866 ) ) ;
#16097 = DIRECTION ( 'NONE',  ( 1.000000000000000000, 0.000000000000000000, 0.000000000000000000 ) ) ;
#16098 = CARTESIAN_POINT ( 'NONE',  ( 120.8143550994449953, 2.935590694028619829, -20.00000000000000000 ) ) ;
#16099 = CARTESIAN_POINT ( 'NONE',  ( 6.500000000000000000, -17.30000000000000071, -2.500000000000000000 ) ) ;
#16100 = DIRECTION ( 'NONE',  ( -0.9730401042858022320, 0.2306359803922080343, 5.959266323858941219E-17 ) ) ;
#16101 = DESIGN_CONTEXT ( 'detailed design', #9124, 'design' ) ;
#16102 = CARTESIAN_POINT ( 'NONE',  ( -22.52506283708769885, 28.95208917575130414, -7.999999999995009325 ) ) ;
#16103 = VERTEX_POINT ( 'NONE', #20685 ) ;
#16104 = DIRECTION ( 'NONE',  ( 1.138590270679730064E-14, 2.220446049251240387E-15, 1.000000000000000000 ) ) ;
#16105 = FACE_OUTER_BOUND ( 'NONE', #6071, .T. ) ;
#16106 = ORIENTED_EDGE ( 'NONE', *, *, #684, .T. ) ;
#16107 = DIRECTION ( 'NONE',  ( -0.2306359803921919083, -0.9730401042858062288, 2.222614453595293935E-13 ) ) ;
#16108 =( BOUNDED_CURVE ( )  B_SPLINE_CURVE ( 2, ( #23030, #13902, #17943 ),
 .UNSPECIFIED., .F., .F. ) 
 B_SPLINE_CURVE_WITH_KNOTS ( ( 3, 3 ),
 ( 0.08763271035584535573, 0.1752654207116860208 ),
 .UNSPECIFIED. ) 
 CURVE ( )  GEOMETRIC_REPRESENTATION_ITEM ( )  RATIONAL_B_SPLINE_CURVE ( ( 1.077350269189624843, 1.077350269189622844, 1.000000000000000000 ) ) 
 REPRESENTATION_ITEM ( '' )  );
#16109 = ORIENTED_EDGE ( 'NONE', *, *, #18232, .T. ) ;
#16110 = VERTEX_POINT ( 'NONE', #17003 ) ;
#16111 = DATE_AND_TIME ( #23229, #3473 ) ;
#16112 = DIRECTION ( 'NONE',  ( 0.000000000000000000, 0.000000000000000000, -1.000000000000000000 ) ) ;
#16113 = ORIENTED_EDGE ( 'NONE', *, *, #1852, .T. ) ;
#16114 = CARTESIAN_POINT ( 'NONE',  ( -14.10663218835320087, 21.82654748245090204, -2.500000000000059952 ) ) ;
#16115 = PERSON_AND_ORGANIZATION_ROLE ( 'design_supplier' ) ;
#16116 = PRODUCT_DEFINITION_SHAPE ( 'NONE', 'NONE',  #9386 ) ;
#16117 = PERSON_AND_ORGANIZATION ( #10805, #20172 ) ;
#16118 = CARTESIAN_POINT ( 'NONE',  ( 120.8143550994449953, 2.935590694028619829, -13.00000000000000000 ) ) ;
#16119 = CIRCLE ( 'NONE', #182, 2.500000000000000444 ) ;
#16120 = CARTESIAN_POINT ( 'NONE',  ( 43.84267580286685018, -31.09999999999999787, -21.50000000000000000 ) ) ;
#16121 = ORIENTED_EDGE ( 'NONE', *, *, #13015, .T. ) ;
#16122 = DIRECTION ( 'NONE',  ( 0.2306359803922037599, 0.9730401042858033422, -4.741332172908110825E-18 ) ) ;
#16123 = EDGE_CURVE ( 'NONE', #4401, #7703, #20451, .T. ) ;
#16124 = ORIENTED_EDGE ( 'NONE', *, *, #20454, .F. ) ;
#16125 = DIRECTION ( 'NONE',  ( -1.000000000000000000, -1.869969807519020344E-43, -1.749697687228930073E-14 ) ) ;
#16126 = FACE_OUTER_BOUND ( 'NONE', #10605, .T. ) ;
#16127 = ORIENTED_EDGE ( 'NONE', *, *, #22588, .T. ) ;
#16128 = DIRECTION ( 'NONE',  ( -2.982858504489139758E-17, 2.441916418604790135E-15, 1.000000000000000000 ) ) ;
#16129 = CARTESIAN_POINT ( 'NONE',  ( 42.88107685774368605, 18.83855087449469679, 13.00000000000000000 ) ) ;
#16130 = ORIENTED_EDGE ( 'NONE', *, *, #13062, .T. ) ;
#16131 =( REPRESENTATION_RELATIONSHIP ('NONE','NONE', #19303, #7037 ) REPRESENTATION_RELATIONSHIP_WITH_TRANSFORMATION ( #7105 )SHAPE_REPRESENTATION_RELATIONSHIP( ) );
#16132 = ORIENTED_EDGE ( 'NONE', *, *, #6334, .T. ) ;
#16133 = PERSON_AND_ORGANIZATION ( #11966, #8758 ) ;
#16134 = PERSON ( 'NAUO-PER22', 'UNSPECIFIED', 'UNSPECIFIED', ('UNSPECIFIED'), ('UNSPECIFIED'), ('UNSPECIFIED') ) ;
#16135 = EDGE_LOOP ( 'NONE', ( #17520, #15917 ) ) ;
#16136 = ORIENTED_EDGE ( 'NONE', *, *, #10403, .F. ) ;
#16137 = FACE_OUTER_BOUND ( 'NONE', #11419, .T. ) ;
#16138 = DATE_AND_TIME ( #3663, #13384 ) ;
#16139 = LINE ( 'NONE', #14361, #5920 ) ;
#16140 = APPROVAL_DATE_TIME ( #7245, #14864 ) ;
#16141 =( NAMED_UNIT ( * ) PLANE_ANGLE_UNIT ( ) SI_UNIT ( $, .RADIAN. ) );
#16142 = DIRECTION ( 'NONE',  ( 0.005235963827197880234, -0.9999862922474489491, 6.243106773925901370E-17 ) ) ;
#16143 = EDGE_CURVE ( 'NONE', #15675, #15347, #22080, .T. ) ;
#16144 = EDGE_CURVE ( 'NONE', #20679, #6022, #9421, .T. ) ;
#16145 = APPROVAL_STATUS ( 'not_yet_approved' ) ;
#16146 = AXIS2_PLACEMENT_3D ( 'NONE', #3236, #1445, #21406 ) ;
#16147 = ORIENTED_EDGE ( 'NONE', *, *, #12894, .T. ) ;
#16148 = CYLINDRICAL_SURFACE ( 'NONE', #6871, 9.000000000000001776 ) ;
#16149 = CARTESIAN_POINT ( 'NONE',  ( 33.37436288052550282, -3.059220458576299873, 13.00000000000019895 ) ) ;
#16150 = ORIENTED_EDGE ( 'NONE', *, *, #18394, .F. ) ;
#16151 = CIRCLE ( 'NONE', #14632, 4.750000000000001776 ) ;
#16152 = DIRECTION ( 'NONE',  ( 1.159535895544890222E-14, 2.167612681253619929E-15, 1.000000000000000000 ) ) ;
#16153 = CYLINDRICAL_SURFACE ( 'NONE', #16838, 2.499999999999998668 ) ;
#16154 = DIRECTION ( 'NONE',  ( -3.099353312215989243E-62, 0.000000000000000000, 1.000000000000000000 ) ) ;
#16155 = ORIENTED_EDGE ( 'NONE', *, *, #7347, .T. ) ;
#16156 = VERTEX_POINT ( 'NONE', #843 ) ;
#16157 = CARTESIAN_POINT ( 'NONE',  ( 115.1338136878955964, -20.09158224951067240, 13.00000000000000000 ) ) ;
#16158 = ORIENTED_EDGE ( 'NONE', *, *, #14842, .T. ) ;
#16159 = PERSON ( 'NAUO-PER40', 'UNSPECIFIED', 'UNSPECIFIED', ('UNSPECIFIED'), ('UNSPECIFIED'), ('UNSPECIFIED') ) ;
#16160 = EDGE_CURVE ( 'NONE', #5502, #13450, #13102, .T. ) ;
#16161 = APPROVAL_STATUS ( 'not_yet_approved' ) ;
#16162 = VERTEX_POINT ( 'NONE', #14869 ) ;
#16163 = VERTEX_POINT ( 'NONE', #9539 ) ;
#16164 = CARTESIAN_POINT ( 'NONE',  ( 114.9904400984930106, 13.05151942359559847, 2.909781424016149503E-14 ) ) ;
#16165 = CARTESIAN_POINT ( 'NONE',  ( -62.75803838139569280, -21.82899804532949872, -5.120040859376149973E-15 ) ) ;
#16166 = CARTESIAN_POINT ( 'NONE',  ( -20.00000000397129796, 22.95208919256900160, 6.500000000004299672 ) ) ;
#16167 = DATE_AND_TIME ( #14849, #11088 ) ;
#16168 = CARTESIAN_POINT ( 'NONE',  ( -68.71210320717760567, 12.64039918458589895, 4.433884350144319916E-15 ) ) ;
#16169 = AXIS2_PLACEMENT_3D ( 'NONE', #12575, #7689, #11388 ) ;
#16170 = FACE_OUTER_BOUND ( 'NONE', #18366, .T. ) ;
#16171 = VECTOR ( 'NONE', #17087, 1000.000000000000227 ) ;
#16172 = SHAPE_REPRESENTATION_RELATIONSHIP ( 'NONE' , 'NONE' ,  #10375, #16174 ) ;
#16173 = EDGE_LOOP ( 'NONE', ( #6981, #15409, #19676, #22145 ) ) ;
#16174 = ADVANCED_BREP_SHAPE_REPRESENTATION ( '', ( #17306, #12739 ), #4017 ) ;
#16175 = LINE ( 'NONE', #3596, #4868 ) ;
#16176 = ADVANCED_FACE ( 'NONE', ( #5963 ), #21982, .F. ) ;
#16177 = DATE_AND_TIME ( #5491, #13334 ) ;
#16178 = CARTESIAN_POINT ( 'NONE',  ( -20.00000000000000000, -20.00000000000000000, 0.000000000000000000 ) ) ;
#16179 = CARTESIAN_POINT ( 'NONE',  ( 39.27359436029429673, 22.26288585089420025, -13.00000000000049916 ) ) ;
#16180 = CC_DESIGN_DATE_AND_TIME_ASSIGNMENT ( #16714, #22179, ( #3831 ) ) ;
#16181 = FACE_BOUND ( 'NONE', #812, .T. ) ;
#16182 = AXIS2_PLACEMENT_3D ( 'NONE', #5177, #12334, #1010 ) ;
#16183 = LINE ( 'NONE', #12974, #641 ) ;
#16184 = APPROVAL ( #12391, 'UNSPECIFIED' ) ;
#16185 = AXIS2_PLACEMENT_3D ( 'NONE', #10463, #14231, #8659 ) ;
#16186 = CIRCLE ( 'NONE', #10913, 2.009239999999998805 ) ;
#16187 = DIRECTION ( 'NONE',  ( 0.000000000000000000, -4.196234823359475661E-16, -1.000000000000000000 ) ) ;
#16188 = ORIENTED_EDGE ( 'NONE', *, *, #2577, .T. ) ;
#16189 = CARTESIAN_POINT ( 'NONE',  ( 36.07092311366584880, 11.78608357701223852, 8.759424124907040365 ) ) ;
#16190 = ADVANCED_FACE ( 'NONE', ( #11340 ), #2520, .F. ) ;
#16191 = ADVANCED_FACE ( 'NONE', ( #6077, #3951, #11580 ), #11224, .F. ) ;
#16192 = VERTEX_POINT ( 'NONE', #9781 ) ;
#16193 = DIRECTION ( 'NONE',  ( 0.9730401042858036753, -0.2306359803922031493, -5.959266323858673745E-17 ) ) ;
#16194 = LINE ( 'NONE', #23426, #10621 ) ;
#16195 = VERTEX_POINT ( 'NONE', #18690 ) ;
#16196 = CARTESIAN_POINT ( 'NONE',  ( 102.2474456857739966, -6.023754975411469204, 3.510479034365399954E-14 ) ) ;
#16197 = ORIENTED_EDGE ( 'NONE', *, *, #20493, .T. ) ;
#16198 = FACE_OUTER_BOUND ( 'NONE', #12367, .T. ) ;
#16199 = CIRCLE ( 'NONE', #13176, 2.749999999999999112 ) ;
#16200 = PERSON_AND_ORGANIZATION_ROLE ( 'design_supplier' ) ;
#16201 = LINE ( 'NONE', #8731, #19628 ) ;
#16202 = CONICAL_SURFACE ( 'NONE', #20002, 1.154700538379250796, 1.047197551196598297 ) ;
#16203 = VECTOR ( 'NONE', #17118, 1000.000000000000000 ) ;
#16204 =( NAMED_UNIT ( * ) SI_UNIT ( $, .STERADIAN. ) SOLID_ANGLE_UNIT ( ) );
#16205 = CARTESIAN_POINT ( 'NONE',  ( -1.262685242559879909E-14, -17.30000000000000071, 2.500000000000000000 ) ) ;
#16206 = CARTESIAN_POINT ( 'NONE',  ( 36.33124047800322387, 11.14167175084450889, -27.55602540378493970 ) ) ;
#16207 = EDGE_CURVE ( 'NONE', #965, #22020, #5410, .T. ) ;
#16208 = CARTESIAN_POINT ( 'NONE',  ( 0.000000000000000000, 0.000000000000000000, 0.000000000000000000 ) ) ;
#16209 = CIRCLE ( 'NONE', #2171, 2.499999999999999112 ) ;
#16210 = DIRECTION ( 'NONE',  ( -0.8823529412199658806, 0.4705882352125641543, 1.991462550421374292E-13 ) ) ;
#16211 = DIRECTION ( 'NONE',  ( -0.9997651245102240347, -0.02167246670447264822, 0.000000000000000000 ) ) ;
#16212 = CARTESIAN_POINT ( 'NONE',  ( -20.00000000397270128, 22.95208919257349933, 8.000000000004460432 ) ) ;
#16213 = LINE ( 'NONE', #5634, #9528 ) ;
#16214 = VERTEX_POINT ( 'NONE', #22335 ) ;
#16215 = AXIS2_PLACEMENT_3D ( 'NONE', #7652, #14493, #9148 ) ;
#16216 = DIRECTION ( 'NONE',  ( -0.9730401042858036753, 0.2306359803922028995, 1.292536702527485292E-16 ) ) ;
#16217 = DIRECTION ( 'NONE',  ( -0.9999862922464843873, -0.005235964011397749134, 0.000000000000000000 ) ) ;
#16218 = EDGE_CURVE ( 'NONE', #9054, #15865, #7867, .T. ) ;
#16220 = VERTEX_POINT ( 'NONE', #20800 ) ;
#16219 = EDGE_CURVE ( 'NONE', #23127, #17030, #7989, .T. ) ;
#16221 = AXIS2_PLACEMENT_3D ( 'NONE', #7314, #7428, #23327 ) ;
#16222 = AXIS2_PLACEMENT_3D ( 'NONE', #22701, #18930, #1089 ) ;
#16223 = COORDINATED_UNIVERSAL_TIME_OFFSET ( 0, 0, .AHEAD. ) ;
#16224 = CARTESIAN_POINT ( 'NONE',  ( 35.59419854219520118, 9.774809681453278998, 21.49999999999999289 ) ) ;
#16225 = AXIS2_PLACEMENT_3D ( 'NONE', #21894, #39, #12663 ) ;
#16226 = ORIENTED_EDGE ( 'NONE', *, *, #1682, .F. ) ;
#16227 = CALENDAR_DATE ( 2026, 31, 10 ) ;
#16228 = DIRECTION ( 'NONE',  ( -0.005235963827110211646, 0.9999862922474493931, 0.000000000000000000 ) ) ;
#16229 = ORIENTED_EDGE ( 'NONE', *, *, #17270, .T. ) ;
#16230 = DIRECTION ( 'NONE',  ( 3.099353312215989243E-62, -9.554441540188157279E-93, -1.000000000000000000 ) ) ;
#16231 = APPROVAL_ROLE ( '' ) ;
#16232 = AXIS2_PLACEMENT_3D ( 'NONE', #8997, #16336, #8757 ) ;
#16233 = PERSON_AND_ORGANIZATION ( #16134, #4993 ) ;
#16234 = CARTESIAN_POINT ( 'NONE',  ( 0.5868595415223712974, -1.010778882616216512, 21.49999999999999289 ) ) ;
#16235 = ADVANCED_FACE ( 'NONE', ( #1191 ), #2875, .T. ) ;
#16236 = DIRECTION ( 'NONE',  ( 0.9730401042858035643, -0.2306359803922031215, 2.740969466505752002E-16 ) ) ;
#16237 = VERTEX_POINT ( 'NONE', #2983 ) ;
#16238 = DIRECTION ( 'NONE',  ( -0.9997648975362222190, -0.02168293463503410262, 0.000000000000000000 ) ) ;
#16239 = ORIENTED_EDGE ( 'NONE', *, *, #11766, .F. ) ;
#16240 =( BOUNDED_CURVE ( )  B_SPLINE_CURVE ( 2, ( #3195, #5204, #8551 ),
 .UNSPECIFIED., .F., .F. ) 
 B_SPLINE_CURVE_WITH_KNOTS ( ( 3, 3 ),
 ( 0.000000000000000000, 0.5842180690389588982 ),
 .UNSPECIFIED. ) 
 CURVE ( )  GEOMETRIC_REPRESENTATION_ITEM ( )  RATIONAL_B_SPLINE_CURVE ( ( 1.000000000000000000, 1.154700538379249908, 1.000000000000000000 ) ) 
 REPRESENTATION_ITEM ( '' )  );
#16241 = LINE ( 'NONE', #23354, #19593 ) ;
#16242 = LINE ( 'NONE', #12357, #20164 ) ;
#16243 = CARTESIAN_POINT ( 'NONE',  ( -20.00000000000000000, -22.50000000000000000, 5.000000000004565237 ) ) ;
#16244 = VERTEX_POINT ( 'NONE', #15453 ) ;
#16245 = EDGE_CURVE ( 'NONE', #10657, #17474, #12038, .T. ) ;
#16246 = ADVANCED_FACE ( 'NONE', ( #22685 ), #11114, .F. ) ;
#16247 = CARTESIAN_POINT ( 'NONE',  ( -20.00000000000000000, -20.00000000000000000, 5.000000000000000000 ) ) ;
#16248 = CARTESIAN_POINT ( 'NONE',  ( 34.89491389100820129, 23.30074776265919922, 13.00000000000000000 ) ) ;
#16249 = VERTEX_POINT ( 'NONE', #6430 ) ;
#16250 = COORDINATED_UNIVERSAL_TIME_OFFSET ( 0, 0, .AHEAD. ) ;
#16251 = ORIENTED_EDGE ( 'NONE', *, *, #13716, .F. ) ;
#16252 = ORIENTED_EDGE ( 'NONE', *, *, #21107, .F. ) ;
#16253 = CARTESIAN_POINT ( 'NONE',  ( -32.65701080836369385, 9.273987487686079945, -5.000000000000000000 ) ) ;
#16254 = AXIS2_PLACEMENT_3D ( 'NONE', #9346, #14804, #17908 ) ;
#16255 = PERSON_AND_ORGANIZATION_ROLE ( 'classification_officer' ) ;
#16256 = DIRECTION ( 'NONE',  ( -2.350988701644575146E-39, 1.000000000000000000, -9.249330715586770885E-11 ) ) ;
#16257 = APPROVAL_ROLE ( '' ) ;
#16258 = CARTESIAN_POINT ( 'NONE',  ( 53.15246078658950069, 27.48624099592299785, -2.283499999999966779 ) ) ;
#16259 = APPLICATION_CONTEXT ( 'configuration controlled 3d designs of mechanical parts and assemblies' ) ;
#16260 = CARTESIAN_POINT ( 'NONE',  ( 37.13840842239409312, 23.31972727237320342, -11.00000000000049738 ) ) ;
#16261 = CC_DESIGN_DATE_AND_TIME_ASSIGNMENT ( #16177, #17982, ( #20770 ) ) ;
#16262 = APPROVAL_DATE_TIME ( #12373, #22338 ) ;
#16263 = ORIENTED_EDGE ( 'NONE', *, *, #7510, .F. ) ;
#16264 = FACE_OUTER_BOUND ( 'NONE', #22578, .T. ) ;
#16265 = CARTESIAN_POINT ( 'NONE',  ( -19.49999999982360066, -0.1021026942259639914, 2.500000000000000000 ) ) ;
#16266 = ORIENTED_EDGE ( 'NONE', *, *, #3238, .F. ) ;
#16267 = CARTESIAN_POINT ( 'NONE',  ( -20.22823963489775068, 17.95730124203003442, 5.000000000004473755 ) ) ;
#16268 = DIRECTION ( 'NONE',  ( 0.8846153846154072298, -0.4663213712685009837, 0.000000000000000000 ) ) ;
#16269 = CARTESIAN_POINT ( 'NONE',  ( 30.72899802076620190, 10.92798958341440141, -1.853207297523799892E-13 ) ) ;
#16270 = VERTEX_POINT ( 'NONE', #5004 ) ;
#16271 = ORIENTED_EDGE ( 'NONE', *, *, #11879, .F. ) ;
#16273 = DIRECTION ( 'NONE',  ( 0.000000000000000000, 0.000000000000000000, 1.000000000000000000 ) ) ;
#16272 = AXIS2_PLACEMENT_3D ( 'NONE', #12676, #19910, #4102 ) ;
#16274 = EDGE_LOOP ( 'NONE', ( #9152, #4146, #7115, #18691 ) ) ;
#16275 = APPROVAL_DATE_TIME ( #21740, #4742 ) ;
#16276 = VERTEX_POINT ( 'NONE', #20914 ) ;
#16277 = ORIENTED_EDGE ( 'NONE', *, *, #21002, .T. ) ;
#16278 = LINE ( 'NONE', #12840, #5837 ) ;
#16279 = DIRECTION ( 'NONE',  ( 1.000000000000000000, -2.270069654138870255E-15, 3.099353312215988811E-62 ) ) ;
#16280 = APPROVAL_DATE_TIME ( #18073, #6025 ) ;
#16281 = DIRECTION ( 'NONE',  ( 0.1630842657209384816, 0.6880432561069583786, -0.7071067811865453523 ) ) ;
#16282 = EDGE_CURVE ( 'NONE', #2031, #9640, #2754, .T. ) ;
#16283 = CARTESIAN_POINT ( 'NONE',  ( 0.000000000000000000, 0.000000000000000000, 0.000000000000000000 ) ) ;
#16284 = COORDINATED_UNIVERSAL_TIME_OFFSET ( 0, 0, .AHEAD. ) ;
#16285 = VECTOR ( 'NONE', #375, 1000.000000000000000 ) ;
#16286 = ORIENTED_EDGE ( 'NONE', *, *, #4179, .F. ) ;
#16287 = CYLINDRICAL_SURFACE ( 'NONE', #1444, 2.500000000000000444 ) ;
#16288 = SECURITY_CLASSIFICATION_LEVEL ( 'unclassified' ) ;
#16289 = LINE ( 'NONE', #7057, #13659 ) ;
#16290 = DIRECTION ( 'NONE',  ( -0.9730401042858035643, 0.2306359803922028717, 6.126766849694256332E-17 ) ) ;
#16291 = CARTESIAN_POINT ( 'NONE',  ( -17.24999999999766587, -20.00000000000000000, 8.500000000003927525 ) ) ;
#16292 = CARTESIAN_POINT ( 'NONE',  ( 58.73439644601030096, 17.65016624305009785, -13.00000000000049916 ) ) ;
#16293 = CARTESIAN_POINT ( 'NONE',  ( -25.44812980900369936, 25.46511081327010118, 3.749999999999940048 ) ) ;
#16294 = VERTEX_POINT ( 'NONE', #13674 ) ;
#16295 = CARTESIAN_POINT ( 'NONE',  ( 34.08722126974237199, 11.19602313317669307, 8.940971698096578990 ) ) ;
#16296 = UNCERTAINTY_MEASURE_WITH_UNIT (LENGTH_MEASURE( 1.000000000000000082E-05 ), #3501, 'distance_accuracy_value', 'NONE');
#16297 = PRODUCT_DEFINITION_SHAPE ( 'NONE', 'NONE',  #20770 ) ;
#16298 = VERTEX_POINT ( 'NONE', #10488 ) ;
#16299 = DIRECTION ( 'NONE',  ( -0.9997648975362233292, -0.02168293463498010415, 0.000000000000000000 ) ) ;
#16300 = DIRECTION ( 'NONE',  ( -2.269700743865584947E-13, -2.220446049247695246E-15, -1.000000000000000000 ) ) ;
#16301 = AXIS2_PLACEMENT_3D ( 'NONE', #8029, #18952, #17291 ) ;
#16302 = ORIENTED_EDGE ( 'NONE', *, *, #15797, .F. ) ;
#16303 = VECTOR ( 'NONE', #9041, 1000.000000000000000 ) ;
#16304 = LINE ( 'NONE', #7531, #4290 ) ;
#16305 = EDGE_CURVE ( 'NONE', #21743, #18309, #12274, .T. ) ;
#16306 = ORIENTED_EDGE ( 'NONE', *, *, #9494, .T. ) ;
#16307 = CARTESIAN_POINT ( 'NONE',  ( -22.52506282043049879, 26.45208917575140006, 6.750000000004490630 ) ) ;
#16308 = CALENDAR_DATE ( 2026, 31, 10 ) ;
#16309 = DIRECTION ( 'NONE',  ( -0.9730401042858035643, 0.2306359803922028717, 5.432877459303547053E-17 ) ) ;
#16310 = AXIS2_PLACEMENT_3D ( 'NONE', #6945, #14174, #5143 ) ;
#16311 = CC_DESIGN_DATE_AND_TIME_ASSIGNMENT ( #4813, #21191, ( #1200 ) ) ;
#16312 = VECTOR ( 'NONE', #18440, 1000.000000000000000 ) ;
#16313 = CARTESIAN_POINT ( 'NONE',  ( 36.10037903421270755, -9.768828191507928693, 2.700000000000049916 ) ) ;
#16314 = EDGE_CURVE ( 'NONE', #19758, #16103, #20954, .T. ) ;
#16315 = EDGE_CURVE ( 'NONE', #2314, #12703, #4659, .T. ) ;
#16316 = DIRECTION ( 'NONE',  ( 0.2306359803922025387, 0.9730401042858035643, -4.741332172907917461E-18 ) ) ;
#16317 = CC_DESIGN_APPROVAL ( #4742, ( #8383 ) ) ;
#16318 = DIRECTION ( 'NONE',  ( -0.9730401042858035643, 0.2306359803922028717, 5.959266323858677443E-17 ) ) ;
#16319 = DIRECTION ( 'NONE',  ( 0.000000000000000000, 0.000000000000000000, -1.000000000000000000 ) ) ;
#16320 = CYLINDRICAL_SURFACE ( 'NONE', #19570, 2.750000000000000000 ) ;
#16321 = DESIGN_CONTEXT ( 'detailed design', #924, 'design' ) ;
#16322 = DIRECTION ( 'NONE',  ( 1.000000000000000000, 9.249025156865542385E-11, -2.269596547736322531E-13 ) ) ;
#16323 = CARTESIAN_POINT ( 'NONE',  ( -16.50000000000000000, -20.00000000000000000, -2.500000000000000000 ) ) ;
#16324 = DIRECTION ( 'NONE',  ( 0.2306359803922080898, 0.9730401042858024541, -2.572202231434325988E-16 ) ) ;
#16325 = CIRCLE ( 'NONE', #4199, 3.499999999999999556 ) ;
#16326 = VERTEX_POINT ( 'NONE', #22930 ) ;
#16327 = EDGE_LOOP ( 'NONE', ( #5100, #14356 ) ) ;
#16328 = LINE ( 'NONE', #3519, #20955 ) ;
#16329 = CARTESIAN_POINT ( 'NONE',  ( 37.01481097301077483, 22.79827665208023646, -15.00000000000051159 ) ) ;
#16330 = ORIENTED_EDGE ( 'NONE', *, *, #18037, .F. ) ;
#16331 = COORDINATED_UNIVERSAL_TIME_OFFSET ( 0, 0, .AHEAD. ) ;
#16332 = DIRECTION ( 'NONE',  ( 0.7071067811865475727, 0.000000000000000000, -0.7071067811865474617 ) ) ;
#16333 = ADVANCED_FACE ( 'NONE', ( #11933 ), #17257, .T. ) ;
#16334 = EDGE_LOOP ( 'NONE', ( #15577, #14405 ) ) ;
#16335 = APPROVAL_PERSON_ORGANIZATION ( #22911, #10713, #12365 ) ;
#16336 = DIRECTION ( 'NONE',  ( 0.000000000000000000, 0.000000000000000000, 1.000000000000000000 ) ) ;
#16337 = APPROVAL_PERSON_ORGANIZATION ( #19140, #17068, #1049 ) ;
#16338 = PERSON_AND_ORGANIZATION_ROLE ( 'classification_officer' ) ;
#16339 = CC_DESIGN_PERSON_AND_ORGANIZATION_ASSIGNMENT ( #3770, #18046, ( #10711 ) ) ;
#16340 = AXIS2_PLACEMENT_3D ( 'NONE', #12804, #20039, #4007 ) ;
#16341 = APPROVAL ( #11429, 'UNSPECIFIED' ) ;
#16342 = DATE_AND_TIME ( #18255, #12961 ) ;
#16343 = FACE_OUTER_BOUND ( 'NONE', #9547, .T. ) ;
#16344 = ADVANCED_FACE ( 'NONE', ( #10251, #6683 ), #19374, .F. ) ;
#16345 = ADVANCED_FACE ( 'NONE', ( #13914 ), #13559, .F. ) ;
#16346 = APPROVAL ( #11765, 'UNSPECIFIED' ) ;
#16347 = FACE_OUTER_BOUND ( 'NONE', #5848, .T. ) ;
#16348 = EDGE_LOOP ( 'NONE', ( #6860, #767, #1271, #7566, #3200 ) ) ;
#16349 = LINE ( 'NONE', #8898, #5635 ) ;
#16350 = LOCAL_TIME ( 14, 11, 27.00000000000000000, #21704 ) ;
#16351 = EDGE_LOOP ( 'NONE', ( #9671, #14806 ) ) ;
#16352 = LOCAL_TIME ( 14, 11, 27.00000000000000000, #12058 ) ;
#16353 = DIRECTION ( 'NONE',  ( 1.000000000000000000, 9.248967332749676061E-11, -1.142026288351397951E-14 ) ) ;
#16355 = AXIS2_PLACEMENT_3D ( 'NONE', #13993, #1287, #4968 ) ;
#16354 = DIRECTION ( 'NONE',  ( 5.798605125234323991E-17, -1.374421231021384554E-17, 1.000000000000000000 ) ) ;
#16356 = PLANE ( 'NONE',  #786 ) ;
#16357 = EDGE_LOOP ( 'NONE', ( #6019, #11867 ) ) ;
#16358 = APPROVAL_STATUS ( 'not_yet_approved' ) ;
#16359 = DIRECTION ( 'NONE',  ( 1.534091707905539846E-93, -1.630753928186650048E-31, 1.000000000000000000 ) ) ;
#16360 = LOCAL_TIME ( 14, 11, 27.00000000000000000, #4380 ) ;
#16361 = EDGE_LOOP ( 'NONE', ( #6413, #11897, #15225, #1048 ) ) ;
#16362 = APPROVAL_STATUS ( 'not_yet_approved' ) ;
#16363 = EDGE_CURVE ( 'NONE', #252, #15338, #960, .T. ) ;
#16364 = ORIENTED_EDGE ( 'NONE', *, *, #19771, .F. ) ;
#16365 = ORIENTED_EDGE ( 'NONE', *, *, #6902, .F. ) ;
#16366 = DIRECTION ( 'NONE',  ( 0.005235964026270697493, -0.9999862922464064496, 2.442051063555178886E-15 ) ) ;
#16367 = APPROVAL_DATE_TIME ( #319, #2995 ) ;
#16368 = EDGE_CURVE ( 'NONE', #21302, #6814, #13412, .T. ) ;
#16369 = PRODUCT_DEFINITION_FORMATION_WITH_SPECIFIED_SOURCE ( 'ANY', '', #14223, .NOT_KNOWN. ) ;
#16370 = CARTESIAN_POINT ( 'NONE',  ( 35.51881378817719792, 11.33423814690520004, -29.25000000000050093 ) ) ;
#16371 = CALENDAR_DATE ( 2026, 31, 10 ) ;
#16372 = LINE ( 'NONE', #11188, #2858 ) ;
#16373 = VECTOR ( 'NONE', #15485, 1000.000000000000000 ) ;
#16374 = EDGE_CURVE ( 'NONE', #19937, #3422, #1314, .T. ) ;
#16375 = ADVANCED_FACE ( 'NONE', ( #23042 ), #6797, .F. ) ;
#16376 =( BOUNDED_CURVE ( )  B_SPLINE_CURVE ( 2, ( #11714, #14776, #6237 ),
 .UNSPECIFIED., .F., .F. ) 
 B_SPLINE_CURVE_WITH_KNOTS ( ( 3, 3 ),
 ( 0.000000000000000000, 0.5842180690389578990 ),
 .UNSPECIFIED. ) 
 CURVE ( )  GEOMETRIC_REPRESENTATION_ITEM ( )  RATIONAL_B_SPLINE_CURVE ( ( 1.000000000000000000, 1.154700538379249908, 1.000000000000000000 ) ) 
 REPRESENTATION_ITEM ( '' )  );
#16377 = SHAPE_REPRESENTATION_RELATIONSHIP ( 'NONE' , 'NONE' ,  #22194, #16713 ) ;
#16378 = LOCAL_TIME ( 14, 11, 27.00000000000000000, #20729 ) ;
#16379 = CARTESIAN_POINT ( 'NONE',  ( 28.87791045744280183, 0.08327042291992099721, 12.50000000000020073 ) ) ;
#16380 = PERSON_AND_ORGANIZATION ( #11966, #8758 ) ;
#16381 = ORIENTED_EDGE ( 'NONE', *, *, #19122, .T. ) ;
#16382 = FACE_OUTER_BOUND ( 'NONE', #13225, .T. ) ;
#16383 = VERTEX_POINT ( 'NONE', #7149 ) ;
#16384 = LOCAL_TIME ( 14, 11, 27.00000000000000000, #231 ) ;
#16385 = CARTESIAN_POINT ( 'NONE',  ( 37.67179450110460692, -4.077824265976569329, -13.00000000000000000 ) ) ;
#16386 = DIRECTION ( 'NONE',  ( 0.000000000000000000, -1.000000000000000000, 2.286959927910970108E-15 ) ) ;
#16387 = DIRECTION ( 'NONE',  ( 6.123230159571619958E-17, 0.000000000000000000, 1.000000000000000000 ) ) ;
#16388 = ORIENTED_EDGE ( 'NONE', *, *, #18190, .T. ) ;
#16389 = VERTEX_POINT ( 'NONE', #17958 ) ;
#16390 = LINE ( 'NONE', #14620, #9488 ) ;
#16391 = ORIENTED_EDGE ( 'NONE', *, *, #2974, .T. ) ;
#16392 = DATE_AND_TIME ( #19729, #17480 ) ;
#16393 = ORIENTED_EDGE ( 'NONE', *, *, #5138, .F. ) ;
#16394 = CONICAL_SURFACE ( 'NONE', #3499, 2.254620000000000513, 0.7853981633974461696 ) ;
#16395 = EDGE_LOOP ( 'NONE', ( #2131, #20318, #17913, #21528 ) ) ;
#16396 = CARTESIAN_POINT ( 'NONE',  ( 120.8143550994449953, 2.935590694028659797, 13.00000000000000000 ) ) ;
#16397 = FACE_OUTER_BOUND ( 'NONE', #2854, .T. ) ;
#16398 = DIRECTION ( 'NONE',  ( -0.4865200521429014491, 0.1153179901961012555, 0.8660254037844388186 ) ) ;
#16399 = PERSON_AND_ORGANIZATION_ROLE ( 'design_owner' ) ;
#16400 = APPLICATION_CONTEXT ( 'configuration controlled 3d designs of mechanical parts and assemblies' ) ;
#16401 = FACE_OUTER_BOUND ( 'NONE', #23449, .T. ) ;
#16402 = DIRECTION ( 'NONE',  ( -0.04564792618500997101, -0.9989575901083128651, 2.775557561562890562E-15 ) ) ;
#16403 = CIRCLE ( 'NONE', #6952, 0.09999999999999939493 ) ;
#16404 = LOCAL_TIME ( 14, 11, 27.00000000000000000, #13409 ) ;
#16405 = CIRCLE ( 'NONE', #2778, 2.500000000000000444 ) ;
#16406 = ORIENTED_EDGE ( 'NONE', *, *, #5138, .T. ) ;
#16407 = DIRECTION ( 'NONE',  ( -1.000000000000000000, 0.000000000000000000, 6.124317834331790129E-17 ) ) ;
#16408 = PERSON_AND_ORGANIZATION ( #11966, #8758 ) ;
#16409 = ORIENTED_EDGE ( 'NONE', *, *, #9954, .F. ) ;
#16410 = DIRECTION ( 'NONE',  ( -0.1630842657209382041, -0.6880432561069511621, 0.7071067811865524577 ) ) ;
#16411 = DIRECTION ( 'NONE',  ( -0.2306359803922027607, -0.9730401042858035643, 1.407521210652529060E-17 ) ) ;
#16412 = CARTESIAN_POINT ( 'NONE',  ( 36.68523773071988359, 8.745424676169351486, -27.44000000000048445 ) ) ;
#16413 = EDGE_CURVE ( 'NONE', #12652, #746, #10744, .T. ) ;
#16414 = LINE ( 'NONE', #5720, #17348 ) ;
#16415 = CARTESIAN_POINT ( 'NONE',  ( 112.5523895830310011, 2.765522746992189695, 3.181688650527689809E-14 ) ) ;
#16416 = ORIENTED_EDGE ( 'NONE', *, *, #6081, .T. ) ;
#16417 = AXIS2_PLACEMENT_3D ( 'NONE', #19655, #2065, #18003 ) ;
#16418 = CARTESIAN_POINT ( 'NONE',  ( 33.98758127650715721, 8.467323122883840369, 8.849131568618506805 ) ) ;
#16419 = CIRCLE ( 'NONE', #14137, 0.0009999999999996990463 ) ;
#16420 = CC_DESIGN_SECURITY_CLASSIFICATION ( #4302, ( #14534 ) ) ;
#16421 = EDGE_LOOP ( 'NONE', ( #3739, #17809, #19188, #15681 ) ) ;
#16422 = CARTESIAN_POINT ( 'NONE',  ( -20.00000000397400157, 22.95208919257349933, -5.499999999995569766 ) ) ;
#16423 = CARTESIAN_POINT ( 'NONE',  ( -25.64168762722610140, 6.365828311191170208, -3.750000000000000000 ) ) ;
#16424 = EDGE_LOOP ( 'NONE', ( #14500, #5081, #18735, #19002 ) ) ;
#16425 = VECTOR ( 'NONE', #21580, 999.9999999999998863 ) ;
#16426 = CARTESIAN_POINT ( 'NONE',  ( 33.91130781617516732, -0.3602965737505582910, 13.00000000000000355 ) ) ;
#16427 = ADVANCED_BREP_SHAPE_REPRESENTATION ( '', ( #17699, #12739 ), #20868 ) ;
#16428 = ORIENTED_EDGE ( 'NONE', *, *, #16086, .T. ) ;
#16429 = DIRECTION ( 'NONE',  ( -0.9730401042858036753, 0.2306359803922028995, -2.804983810440358801E-16 ) ) ;
#16430 = APPROVAL_DATE_TIME ( #8968, #20397 ) ;
#16431 = CARTESIAN_POINT ( 'NONE',  ( 0.03403376487640639991, -6.499910899608420500, 2.500000000000090150 ) ) ;
#16432 = AXIS2_PLACEMENT_3D ( 'NONE', #13086, #343, #704 ) ;
#16433 = DIRECTION ( 'NONE',  ( -0.2306359803922026497, -0.9730401042858035643, 0.000000000000000000 ) ) ;
#16434 = DIRECTION ( 'NONE',  ( 0.2306359803922080898, 0.9730401042858024541, -2.572202231434325988E-16 ) ) ;
#16435 = DIRECTION ( 'NONE',  ( 0.000000000000000000, 0.000000000000000000, 1.000000000000000000 ) ) ;
#16436 = CIRCLE ( 'NONE', #3549, 4.250000000000001776 ) ;
#16437 = CARTESIAN_POINT ( 'NONE',  ( -14.54830929662900019, 0.3367883020382110293, -7.999999999996749267 ) ) ;
#16438 = AXIS2_PLACEMENT_3D ( 'NONE', #19956, #10954, #2493 ) ;
#16439 = DIRECTION ( 'NONE',  ( 0.9999862922474493931, 0.005235963827108368503, 0.000000000000000000 ) ) ;
#16440 = CARTESIAN_POINT ( 'NONE',  ( 32.64280992401804582, -5.712017147322579369, -12.99999999999999645 ) ) ;
#16441 = ADVANCED_FACE ( 'NONE', ( #3579, #19851, #3787, #14257, #20063, #7383 ), #1664, .T. ) ;
#16442 = CARTESIAN_POINT ( 'NONE',  ( 5.795358483849606834, 14.71364485406434675, -5.628665133555442742E-15 ) ) ;
#16443 = CARTESIAN_POINT ( 'NONE',  ( 39.37089837072279863, 22.23982225285499936, -13.00000000000049916 ) ) ;
#16444 = DIRECTION ( 'NONE',  ( -3.210834492181045054E-17, 2.441916418604790135E-15, 1.000000000000000000 ) ) ;
#16445 = EDGE_LOOP ( 'NONE', ( #15607, #21928, #4884, #18461, #5578, #20831 ) ) ;
#16446 = VERTEX_POINT ( 'NONE', #7261 ) ;
#16447 = PLANE ( 'NONE',  #17565 ) ;
#16448 = DIRECTION ( 'NONE',  ( -0.9730401042858036753, 0.2306359803922023999, -1.110223024625155524E-17 ) ) ;
#16449 = VERTEX_POINT ( 'NONE', #10723 ) ;
#16450 = EDGE_CURVE ( 'NONE', #577, #13906, #16022, .T. ) ;
#16451 = EDGE_CURVE ( 'NONE', #3638, #16709, #8455, .T. ) ;
#16452 = DIRECTION ( 'NONE',  ( 0.005235963827101452160, -0.9999862922474493931, 5.479105319409471602E-16 ) ) ;
#16453 = VECTOR ( 'NONE', #3271, 1000.000000000000114 ) ;
#16454 = ORIENTED_EDGE ( 'NONE', *, *, #5192, .F. ) ;
#16455 = DIRECTION ( 'NONE',  ( -1.159535895544890222E-14, -2.167612681253619929E-15, -1.000000000000000000 ) ) ;
#16456 = PERSON_AND_ORGANIZATION ( #11966, #8758 ) ;
#16457 = TOROIDAL_SURFACE ( 'NONE', #143, 2.600000000000000089, 0.1000000000000000056 ) ;
#16458 = CARTESIAN_POINT ( 'NONE',  ( 36.44304717685047024, 7.885313416653864316, -8.849131568618497923 ) ) ;
#16459 = DATE_TIME_ROLE ( 'classification_date' ) ;
#16460 = CARTESIAN_POINT ( 'NONE',  ( -69.87051617300704720, -0.3658445101694126067, 0.000000000000000000 ) ) ;
#16461 = ORIENTED_EDGE ( 'NONE', *, *, #2678, .F. ) ;
#16462 = DIRECTION ( 'NONE',  ( -0.2306359803922019835, -0.9730401042858037863, 4.163336342344336238E-15 ) ) ;
#16463 = VERTEX_POINT ( 'NONE', #16044 ) ;
#16464 = DIRECTION ( 'NONE',  ( -0.5021071549687909918, 0.8648054144888007722, -3.074521526981951182E-17 ) ) ;
#16465 = EDGE_CURVE ( 'NONE', #5109, #21047, #18062, .T. ) ;
#16466 = VERTEX_POINT ( 'NONE', #23279 ) ;
#16467 = LINE ( 'NONE', #12912, #17319 ) ;
#16468 = DIRECTION ( 'NONE',  ( 0.9730401042858035643, -0.2306359803922028717, -5.959266323858677443E-17 ) ) ;
#16469 = DIRECTION ( 'NONE',  ( -2.829953705592110306E-16, -9.355573283744330345E-16, -1.000000000000000000 ) ) ;
#16470 = ORIENTED_EDGE ( 'NONE', *, *, #1712, .F. ) ;
#16471 = APPROVAL ( #11878, 'UNSPECIFIED' ) ;
#16472 = APPROVAL_ROLE ( '' ) ;
#16473 = APPROVAL ( #4954, 'UNSPECIFIED' ) ;
#16474 = DIRECTION ( 'NONE',  ( 2.982858504489139758E-17, -2.441916418604790135E-15, -1.000000000000000000 ) ) ;
#16475 = ORIENTED_EDGE ( 'NONE', *, *, #13119, .F. ) ;
#16476 = EDGE_CURVE ( 'NONE', #5973, #8304, #7038, .T. ) ;
#16477 = EDGE_CURVE ( 'NONE', #4246, #15256, #5026, .T. ) ;
#16478 = COORDINATED_UNIVERSAL_TIME_OFFSET ( 0, 0, .AHEAD. ) ;
#16479 = ORIENTED_EDGE ( 'NONE', *, *, #12340, .T. ) ;
#16480 = ORIENTED_EDGE ( 'NONE', *, *, #14479, .F. ) ;
#16481 = EDGE_CURVE ( 'NONE', #14815, #16110, #1772, .T. ) ;
#16482 = CARTESIAN_POINT ( 'NONE',  ( 39.97055191974263266, 24.76972652399818742, 13.00000000000000000 ) ) ;
#16483 = EDGE_CURVE ( 'NONE', #6885, #20045, #12254, .T. ) ;
#16484 = APPROVAL_DATE_TIME ( #12815, #7933 ) ;
#16485 = VECTOR ( 'NONE', #18984, 1000.000000000000000 ) ;
#16486 = DIRECTION ( 'NONE',  ( -0.9730401042858032312, 0.2306359803922040375, -1.084982917713590005E-15 ) ) ;
#16487 = APPROVAL_ROLE ( '' ) ;
#16488 = CARTESIAN_POINT ( 'NONE',  ( -25.64168762722610140, 6.365828311191160438, -5.000000000000000000 ) ) ;
#16489 = CYLINDRICAL_SURFACE ( 'NONE', #6193, 2.066999999999997950 ) ;
#16490 = CALENDAR_DATE ( 2026, 31, 10 ) ;
#16491 = EDGE_CURVE ( 'NONE', #13288, #2314, #5772, .T. ) ;
#16492 = PRODUCT_DEFINITION_SHAPE ( 'NONE', 'NONE',  #23500 ) ;
#16493 = ORIENTED_EDGE ( 'NONE', *, *, #21002, .F. ) ;
#16494 = CARTESIAN_POINT ( 'NONE',  ( -58.40964484538829993, -25.30627767975780174, 2.500000000000000000 ) ) ;
#16495 = EDGE_LOOP ( 'NONE', ( #4940, #2765, #22156, #12784, #17236 ) ) ;
#16496 = DIRECTION ( 'NONE',  ( 8.911056267098788616E-18, 1.998401444326210262E-15, 1.000000000000000000 ) ) ;
#16497 = CARTESIAN_POINT ( 'NONE',  ( -58.40964484538829993, -25.30627767975780174, -2.500000000000000000 ) ) ;
#16498 = CARTESIAN_POINT ( 'NONE',  ( 32.64280992401804582, -5.712017147322479005, 13.00000000000000355 ) ) ;
#16499 = ORIENTED_EDGE ( 'NONE', *, *, #21659, .F. ) ;
#16500 = ORIENTED_EDGE ( 'NONE', *, *, #8807, .F. ) ;
#16501 = CARTESIAN_POINT ( 'NONE',  ( 39.27359436029389883, 22.26288585089424998, -13.00000000000030020 ) ) ;
#16502 = ORIENTED_EDGE ( 'NONE', *, *, #18932, .T. ) ;
#16503 = ADVANCED_FACE ( 'NONE', ( #11067 ), #8693, .F. ) ;
#16504 = EDGE_CURVE ( 'NONE', #20385, #21866, #23219, .T. ) ;
#16505 = PERSON_AND_ORGANIZATION ( #11966, #8758 ) ;
#16506 = ORIENTED_EDGE ( 'NONE', *, *, #8520, .T. ) ;
#16507 = ORIENTED_EDGE ( 'NONE', *, *, #16726, .F. ) ;
#16508 = LINE ( 'NONE', #14507, #2036 ) ;
#16509 = DIRECTION ( 'NONE',  ( -1.000000000000000000, 0.000000000000000000, 0.000000000000000000 ) ) ;
#16510 = APPROVAL_ROLE ( '' ) ;
#16511 = DIRECTION ( 'NONE',  ( -0.9999862922474492821, -0.005235963827121822151, 1.187304881134280213E-16 ) ) ;
#16512 = CARTESIAN_POINT ( 'NONE',  ( 30.57814311865390167, -3.583136841840119935, -15.00000000000039968 ) ) ;
#16513 = CIRCLE ( 'NONE', #4392, 3.499999999999998668 ) ;
#16514 =( NAMED_UNIT ( * ) PLANE_ANGLE_UNIT ( ) SI_UNIT ( $, .RADIAN. ) );
#16515 = VERTEX_POINT ( 'NONE', #111 ) ;
#16516 = LINE ( 'NONE', #599, #20032 ) ;
#16517 = CALENDAR_DATE ( 2026, 31, 10 ) ;
#16518 = ADVANCED_FACE ( 'NONE', ( #10956 ), #15922, .T. ) ;
#16519 = ORIENTED_EDGE ( 'NONE', *, *, #12665, .F. ) ;
#16520 = DIRECTION ( 'NONE',  ( 2.269700743865589996E-13, 2.220446049247695246E-15, 1.000000000000000000 ) ) ;
#16521 = CYLINDRICAL_SURFACE ( 'NONE', #6362, 3.499999999999998224 ) ;
#16522 = CYLINDRICAL_SURFACE ( 'NONE', #4797, 0.4000000000000010214 ) ;
#16523 = DIRECTION ( 'NONE',  ( -6.281952996264290168E-17, -4.969341027148640384E-15, -1.000000000000000000 ) ) ;
#16524 = EDGE_CURVE ( 'NONE', #5148, #17755, #4283, .T. ) ;
#16525 = DIRECTION ( 'NONE',  ( -0.9730401042858023430, 0.2306359803922080620, 5.959266323858944916E-17 ) ) ;
#16526 = ORIENTED_EDGE ( 'NONE', *, *, #20324, .T. ) ;
#16527 = FACE_OUTER_BOUND ( 'NONE', #19005, .T. ) ;
#16528 = ADVANCED_FACE ( 'NONE', ( #19723 ), #14539, .F. ) ;
#16529 =( GEOMETRIC_REPRESENTATION_CONTEXT ( 3 ) GLOBAL_UNCERTAINTY_ASSIGNED_CONTEXT ( ( #9184 ) ) GLOBAL_UNIT_ASSIGNED_CONTEXT ( ( #23203, #5161, #16204 ) ) REPRESENTATION_CONTEXT ( 'NONE', 'WORKASPACE' ) );
#16530 = VERTEX_POINT ( 'NONE', #18784 ) ;
#16531 = ORIENTED_EDGE ( 'NONE', *, *, #23416, .F. ) ;
#16532 = DIRECTION ( 'NONE',  ( 0.9730401042858034533, -0.2306359803922026774, 1.869849304631839730E-15 ) ) ;
#16533 = CARTESIAN_POINT ( 'NONE',  ( 34.20600149872029760, 10.48923880214159965, -29.25000000000050093 ) ) ;
#16534 = ORIENTED_EDGE ( 'NONE', *, *, #13043, .F. ) ;
#16535 = CARTESIAN_POINT ( 'NONE',  ( 35.11747397072458199, 7.763535785894707608, 8.759424124906642461 ) ) ;
#16536 = AXIS2_PLACEMENT_3D ( 'NONE', #16989, #18673, #13316 ) ;
#16537 = ORIENTED_EDGE ( 'NONE', *, *, #945, .F. ) ;
#16538 = CARTESIAN_POINT ( 'NONE',  ( 114.0804991654443796, -24.53545640578393261, 13.00000000000000000 ) ) ;
#16539 = COORDINATED_UNIVERSAL_TIME_OFFSET ( 0, 0, .AHEAD. ) ;
#16540 = DIRECTION ( 'NONE',  ( -2.829953705592110306E-16, -9.355573283744330345E-16, -1.000000000000000000 ) ) ;
#16541 = DIRECTION ( 'NONE',  ( -0.9730401042858024541, 0.2306359803922080898, 5.959266323858942451E-17 ) ) ;
#16542 = DIRECTION ( 'NONE',  ( 0.005235963827110361700, -0.9999862922474493931, 0.000000000000000000 ) ) ;
#16543 = APPROVAL_STATUS ( 'not_yet_approved' ) ;
#16544 = VECTOR ( 'NONE', #14462, 999.9999999999998863 ) ;
#16545 = AXIS2_PLACEMENT_3D ( 'NONE', #14397, #3357, #7060 ) ;
#16546 = CARTESIAN_POINT ( 'NONE',  ( -16.50000000000000000, -20.00000000000000711, 2.500000000000000000 ) ) ;
#16547 = LINE ( 'NONE', #3380, #9395 ) ;
#16548 = CC_DESIGN_DATE_AND_TIME_ASSIGNMENT ( #7281, #19516, ( #8771 ) ) ;
#16549 = DIRECTION ( 'NONE',  ( 0.000000000000000000, 0.000000000000000000, 1.000000000000000000 ) ) ;
#16550 = CARTESIAN_POINT ( 'NONE',  ( 37.03119170130820237, 10.20498483259830280, 27.44000000000020378 ) ) ;
#16551 = LINE ( 'NONE', #46, #22121 ) ;
#16552 = CARTESIAN_POINT ( 'NONE',  ( -23.49917714535037661, 22.87619892134627975, -2.500000000000039968 ) ) ;
#16553 = ORIENTED_EDGE ( 'NONE', *, *, #5625, .T. ) ;
#16554 = ORIENTED_EDGE ( 'NONE', *, *, #20430, .T. ) ;
#16555 = CARTESIAN_POINT ( 'NONE',  ( -11.24263882182209962, 20.87636639668270178, 2.500000000000000000 ) ) ;
#16556 = CIRCLE ( 'NONE', #12795, 7.599342076785325695 ) ;
#16557 = ORIENTED_EDGE ( 'NONE', *, *, #22563, .T. ) ;
#16558 = CARTESIAN_POINT ( 'NONE',  ( 35.89100945995100034, 24.25134070964849897, 11.00000000000000000 ) ) ;
#16559 = ORIENTED_EDGE ( 'NONE', *, *, #3594, .F. ) ;
#16560 = AXIS2_PLACEMENT_3D ( 'NONE', #9957, #13505, #9835 ) ;
#16561 = CARTESIAN_POINT ( 'NONE',  ( 1.358598381910800010E-16, -1.434096706618689895E-15, 8.874009851233079243E-14 ) ) ;
#16562 = CONICAL_SURFACE ( 'NONE', #6340, 2.254620000000000513, 0.7853981633974461696 ) ;
#16563 = COORDINATED_UNIVERSAL_TIME_OFFSET ( 0, 0, .AHEAD. ) ;
#16564 = DIRECTION ( 'NONE',  ( -2.196377653365445055E-14, -1.228149275973193960E-30, -1.000000000000000000 ) ) ;
#16565 = ADVANCED_FACE ( 'NONE', ( #7725 ), #333, .F. ) ;
#16566 = DIRECTION ( 'NONE',  ( 0.000000000000000000, 0.000000000000000000, -1.000000000000000000 ) ) ;
#16567 = EDGE_LOOP ( 'NONE', ( #16155, #6775 ) ) ;
#16568 = AXIS2_PLACEMENT_3D ( 'NONE', #19721, #3448, #7259 ) ;
#16569 = CARTESIAN_POINT ( 'NONE',  ( 122.4288069621910040, 9.746871424029270869, 10.02499999999999858 ) ) ;
#16570 = ORIENTED_EDGE ( 'NONE', *, *, #16646, .F. ) ;
#16571 = FACE_OUTER_BOUND ( 'NONE', #7097, .T. ) ;
#16572 = EDGE_CURVE ( 'NONE', #2347, #2950, #7706, .T. ) ;
#16573 = CIRCLE ( 'NONE', #20759, 0.3999999999999982458 ) ;
#16574 = VECTOR ( 'NONE', #18465, 1000.000000000000114 ) ;
#16575 = VECTOR ( 'NONE', #10131, 1000.000000000000000 ) ;
#16576 = ORIENTED_EDGE ( 'NONE', *, *, #3748, .F. ) ;
#16577 = DIRECTION ( 'NONE',  ( -0.8686315144360597928, 0.4954586684361443893, 2.575384811085934765E-17 ) ) ;
#16578 = LINE ( 'NONE', #9472, #11091 ) ;
#16579 = CARTESIAN_POINT ( 'NONE',  ( 36.09092202081949807, 8.115512906978459284, 27.68999999999999773 ) ) ;
#16580 = ORIENTED_EDGE ( 'NONE', *, *, #12740, .F. ) ;
#16581 = EDGE_CURVE ( 'NONE', #341, #17992, #21727, .T. ) ;
#16582 = APPROVAL_DATE_TIME ( #5663, #11838 ) ;
#16583 = DIRECTION ( 'NONE',  ( -0.2306359803922032603, -0.9730401042858035643, 1.407521210652567579E-17 ) ) ;
#16584 = AXIS2_PLACEMENT_3D ( 'NONE', #1731, #10558, #19564 ) ;
#16585 = ORIENTED_EDGE ( 'NONE', *, *, #16745, .T. ) ;
#16586 = PERSON_AND_ORGANIZATION_ROLE ( 'classification_officer' ) ;
#16587 = DIRECTION ( 'NONE',  ( 2.269747459788994803E-13, 2.220446049250310320E-15, 1.000000000000000000 ) ) ;
#16588 = EDGE_LOOP ( 'NONE', ( #19220, #19788, #16750, #15148, #13746 ) ) ;
#16589 = ORIENTED_EDGE ( 'NONE', *, *, #549, .F. ) ;
#16590 = CARTESIAN_POINT ( 'NONE',  ( -0.4837994683632851900, 20.45050988743705744, -3.168006029165976713E-16 ) ) ;
#16591 = DATE_TIME_ROLE ( 'classification_date' ) ;
#16592 = AXIS2_PLACEMENT_3D ( 'NONE', #18474, #2185, #9441 ) ;
#16593 = EDGE_CURVE ( 'NONE', #187, #1337, #10766, .T. ) ;
#16594 = LINE ( 'NONE', #10823, #2891 ) ;
#16595 = ITEM_DEFINED_TRANSFORMATION ( 'NONE', 'NONE', #17461,  #12739 ) ;
#16596 = CARTESIAN_POINT ( 'NONE',  ( -55.82882037092586813, -8.292431354569982815, -7.200000000000000178 ) ) ;
#16597 = CC_DESIGN_PERSON_AND_ORGANIZATION_ASSIGNMENT ( #14298, #4331, ( #5445 ) ) ;
#16598 = CC_DESIGN_PERSON_AND_ORGANIZATION_ASSIGNMENT ( #20810, #11945, ( #13725 ) ) ;
#16599 = LINE ( 'NONE', #20186, #18318 ) ;
#16600 = EDGE_CURVE ( 'NONE', #15535, #12469, #482, .T. ) ;
#16601 = ADVANCED_FACE ( 'NONE', ( #20541 ), #22076, .F. ) ;
#16602 = DATE_AND_TIME ( #18169, #2281 ) ;
#16603 = ORIENTED_EDGE ( 'NONE', *, *, #17226, .T. ) ;
#16604 = VECTOR ( 'NONE', #10070, 1000.000000000000000 ) ;
#16605 = CARTESIAN_POINT ( 'NONE',  ( 38.35918225515318625, -2.116483060172758446, 13.00000000000000000 ) ) ;
#16606 = VERTEX_POINT ( 'NONE', #20311 ) ;
#16607 = LINE ( 'NONE', #2491, #18143 ) ;
#16608 = FACE_OUTER_BOUND ( 'NONE', #18017, .T. ) ;
#16609 = ORIENTED_EDGE ( 'NONE', *, *, #6999, .T. ) ;
#16610 = EDGE_LOOP ( 'NONE', ( #6608, #13098, #7863, #19481 ) ) ;
#16611 = DIRECTION ( 'NONE',  ( -7.283891156702289181E-32, 2.441916418604790135E-15, 1.000000000000000000 ) ) ;
#16612 = EDGE_LOOP ( 'NONE', ( #8256, #6395, #21910, #8988 ) ) ;
#16613 = DATE_TIME_ROLE ( 'creation_date' ) ;
#16614 = ORIENTED_EDGE ( 'NONE', *, *, #17547, .F. ) ;
#16615 = ORIENTED_EDGE ( 'NONE', *, *, #14190, .T. ) ;
#16616 = FACE_OUTER_BOUND ( 'NONE', #2240, .T. ) ;
#16617 = CARTESIAN_POINT ( 'NONE',  ( 34.41917370704150159, 26.49663125198739877, 19.99999999999975131 ) ) ;
#16618 = PERSON_AND_ORGANIZATION ( #11966, #8758 ) ;
#16619 = DIRECTION ( 'NONE',  ( 3.210834492194344756E-17, -2.441916418604790135E-15, -1.000000000000000000 ) ) ;
#16620 = EDGE_CURVE ( 'NONE', #1573, #22534, #11536, .T. ) ;
#16621 = DIRECTION ( 'NONE',  ( 6.124378941434239724E-17, -2.274246353359159970E-33, 1.000000000000000000 ) ) ;
#16622 = CC_DESIGN_DATE_AND_TIME_ASSIGNMENT ( #14950, #18772, ( #1530 ) ) ;
#16624 = CLOSED_SHELL ( 'NONE', ( #22316, #17656, #10322, #3694, #14130, #22354, #11898, #21672, #16565, #17343, #13326, #19880, #16344, #18730, #10847, #13298, #16333, #17922, #10492 ) ) ;
#16623 = CC_DESIGN_PERSON_AND_ORGANIZATION_ASSIGNMENT ( #21611, #3584, ( #3714 ) ) ;
#16625 = VECTOR ( 'NONE', #7225, 1000.000000000000114 ) ;
#16626 = EDGE_CURVE ( 'NONE', #14219, #6893, #20051, .T. ) ;
#16627 = EDGE_CURVE ( 'NONE', #18737, #903, #7489, .T. ) ;
#16628 = VERTEX_POINT ( 'NONE', #12944 ) ;
#16629 = DIRECTION ( 'NONE',  ( 0.000000000000000000, 0.000000000000000000, -1.000000000000000000 ) ) ;
#16630 = APPROVAL_ROLE ( '' ) ;
#16631 = ORIENTED_EDGE ( 'NONE', *, *, #476, .F. ) ;
#16632 = LINE ( 'NONE', #14861, #2273 ) ;
#16633 = CIRCLE ( 'NONE', #17846, 4.250000000000000000 ) ;
#16634 = DIRECTION ( 'NONE',  ( -2.977235988022386522E-185, 9.605990953944227443E-124, 1.000000000000000000 ) ) ;
#16635 = DIRECTION ( 'NONE',  ( -0.9730401042858024541, 0.2306359803922080898, 5.959266323863401980E-17 ) ) ;
#16636 = CARTESIAN_POINT ( 'NONE',  ( 89.62416413250210212, 10.32848256004259824, 12.99999999999970157 ) ) ;
#16637 = DIRECTION ( 'NONE',  ( -1.000000000000000000, -6.662111938308250026E-09, 2.269747459936919981E-13 ) ) ;
#16638 = ORIENTED_EDGE ( 'NONE', *, *, #14874, .T. ) ;
#16639 = DIRECTION ( 'NONE',  ( -0.9730401042858024541, 0.2306359803922080898, 5.959266323858723049E-17 ) ) ;
#16640 = ORIENTED_EDGE ( 'NONE', *, *, #16524, .F. ) ;
#16641 = ORIENTED_EDGE ( 'NONE', *, *, #517, .F. ) ;
#16642 = CARTESIAN_POINT ( 'NONE',  ( -20.00000000000000000, -22.50000000000000000, -4.999999999995464961 ) ) ;
#16643 = PLANE ( 'NONE',  #1854 ) ;
#16644 = VERTEX_POINT ( 'NONE', #7599 ) ;
#16645 = DIRECTION ( 'NONE',  ( 0.9949874374308234071, 0.09999999677421649025, -2.262079412673754937E-13 ) ) ;
#16646 = EDGE_CURVE ( 'NONE', #3305, #4103, #4303, .T. ) ;
#16647 = CARTESIAN_POINT ( 'NONE',  ( 34.40839383886520153, 23.41606575285519654, -13.00000000000049916 ) ) ;
#16648 = APPROVAL_PERSON_ORGANIZATION ( #6580, #14153, #22700 ) ;
#16649 = PERSON_AND_ORGANIZATION ( #8241, #8102 ) ;
#16650 = CIRCLE ( 'NONE', #14392, 4.250000000000000000 ) ;
#16651 = DIRECTION ( 'NONE',  ( -0.9730401042858021210, 0.2306359803922091167, -1.531342102931250897E-15 ) ) ;
#16652 = ADVANCED_FACE ( 'NONE', ( #11311 ), #2373, .F. ) ;
#16653 =( NAMED_UNIT ( * ) PLANE_ANGLE_UNIT ( ) SI_UNIT ( $, .RADIAN. ) );
#16654 = DIRECTION ( 'NONE',  ( -0.9730401042858023430, 0.2306359803922080620, 5.959266323858944916E-17 ) ) ;
#16655 = EDGE_CURVE ( 'NONE', #10873, #1296, #6581, .T. ) ;
#16656 = CARTESIAN_POINT ( 'NONE',  ( 97.29330225143137056, -16.08541248458771022, -13.00000000000000000 ) ) ;
#16657 = APPROVAL_STATUS ( 'not_yet_approved' ) ;
#16658 = EDGE_CURVE ( 'NONE', #5211, #3143, #17583, .T. ) ;
#16659 = CARTESIAN_POINT ( 'NONE',  ( 8.284960688207139157, -8.610885316305260773, -25.00000000000000000 ) ) ;
#16660 = CARTESIAN_POINT ( 'NONE',  ( 28.27870060330370094, -2.444761924717779866, 15.00000000000000000 ) ) ;
#16661 = CARTESIAN_POINT ( 'NONE',  ( 34.49867763533223552, 5.152869186095713872, -26.50000000000047606 ) ) ;
#16662 = DIRECTION ( 'NONE',  ( 5.944927207247209745E-47, 1.000000000000000000, 0.000000000000000000 ) ) ;
#16663 = VECTOR ( 'NONE', #1965, 1000.000000000000000 ) ;
#16664 = CARTESIAN_POINT ( 'NONE',  ( -0.5391976746782148888, 18.33937061236850141, 3.301631463538509622E-17 ) ) ;
#16665 = VECTOR ( 'NONE', #12384, 1000.000000000000000 ) ;
#16666 = DIRECTION ( 'NONE',  ( 0.000000000000000000, 0.000000000000000000, 1.000000000000000000 ) ) ;
#16667 = ORIENTED_EDGE ( 'NONE', *, *, #13716, .T. ) ;
#16668 = ORIENTED_EDGE ( 'NONE', *, *, #12413, .T. ) ;
#16669 = CARTESIAN_POINT ( 'NONE',  ( -16.00004797695772751, -0.08377682083104373567, 2.500000000000089706 ) ) ;
#16670 = LINE ( 'NONE', #22144, #5322 ) ;
#16671 = ORIENTED_EDGE ( 'NONE', *, *, #5781, .T. ) ;
#16672 = VECTOR ( 'NONE', #9295, 999.9999999999998863 ) ;
#16673 = FACE_OUTER_BOUND ( 'NONE', #5387, .T. ) ;
#16674 = EDGE_LOOP ( 'NONE', ( #23194, #1310 ) ) ;
#16675 = DIRECTION ( 'NONE',  ( -0.9730401042858022320, 0.2306359803922080343, 5.959266323858941219E-17 ) ) ;
#16676 = PERSON_AND_ORGANIZATION_ROLE ( 'classification_officer' ) ;
#16677 = CARTESIAN_POINT ( 'NONE',  ( -20.00000000000000000, -20.00000000000000000, 2.500000000000000000 ) ) ;
#16678 = PRODUCT_RELATED_PRODUCT_CATEGORY ( 'detail', '', ( #12718 ) ) ;
#16679 = PRODUCT_DEFINITION_SHAPE ( 'NONE', 'NONE',  #23492 ) ;
#16680 = PRODUCT_DEFINITION_FORMATION_WITH_SPECIFIED_SOURCE ( 'ANY', '', #1697, .NOT_KNOWN. ) ;
#16681 = CALENDAR_DATE ( 2026, 31, 10 ) ;
#16682 = CYLINDRICAL_SURFACE ( 'NONE', #2492, 6.000000000001509015 ) ;
#16683 = AXIS2_PLACEMENT_3D ( 'NONE', #5165, #40, #7193 ) ;
#16684 = CARTESIAN_POINT ( 'NONE',  ( 39.37089837072289811, 22.23982225285509884, 13.00000000000000000 ) ) ;
#16685 = AXIS2_PLACEMENT_3D ( 'NONE', #3983, #9332, #2080 ) ;
#16686 = EDGE_LOOP ( 'NONE', ( #9246, #3223, #10481, #22344 ) ) ;
#16687 = CARTESIAN_POINT ( 'NONE',  ( -1.262685242559879909E-14, -17.30000000000000071, 5.000000000000000000 ) ) ;
#16688 = ORIENTED_EDGE ( 'NONE', *, *, #6286, .T. ) ;
#16690 = AXIS2_PLACEMENT_3D ( 'NONE', #8042, #4591, #15151 ) ;
#16689 = CARTESIAN_POINT ( 'NONE',  ( -14.10663218835320087, 21.82654748245090204, -3.750000000000059508 ) ) ;
#16691 = CARTESIAN_POINT ( 'NONE',  ( -2.499999999999973799, 4.120723506284736299E-15, 2.500000000000000000 ) ) ;
#16692 = EDGE_LOOP ( 'NONE', ( #22624, #8331, #198, #12018 ) ) ;
#16693 = AXIS2_PLACEMENT_3D ( 'NONE', #21967, #3803, #11083 ) ;
#16694 = DIRECTION ( 'NONE',  ( 4.115594265179474725E-36, 2.805478249463630046E-20, 1.000000000000000000 ) ) ;
#16695 = CARTESIAN_POINT ( 'NONE',  ( 34.03002896453743631, 19.65184737158743289, 13.00000000000000000 ) ) ;
#16696 = CARTESIAN_POINT ( 'NONE',  ( 43.40226860240920814, 19.16001186014064572, -13.00000000000000000 ) ) ;
#16697 = ORIENTED_EDGE ( 'NONE', *, *, #14402, .T. ) ;
#16698 = APPLICATION_CONTEXT ( 'configuration controlled 3d designs of mechanical parts and assemblies' ) ;
#16699 = ADVANCED_FACE ( 'NONE', ( #18425, #15076 ), #16974, .T. ) ;
#16700 = SECURITY_CLASSIFICATION ( '', '', #6058 ) ;
#16701 = APPROVAL_ROLE ( '' ) ;
#16702 = DIRECTION ( 'NONE',  ( -0.9730401042858024541, 0.2306359803922080898, 5.959266323858942451E-17 ) ) ;
#16703 = APPROVAL_PERSON_ORGANIZATION ( #12735, #15886, #5362 ) ;
#16704 = VERTEX_POINT ( 'NONE', #16498 ) ;
#16705 = PERSON_AND_ORGANIZATION ( #11966, #8758 ) ;
#16706 = DIRECTION ( 'NONE',  ( 1.000000000000000000, -1.991364888915564904E-60, -2.270069654138870255E-15 ) ) ;
#16707 = CIRCLE ( 'NONE', #2746, 3.499999999999998224 ) ;
#16708 = VERTEX_POINT ( 'NONE', #4394 ) ;
#16709 = VERTEX_POINT ( 'NONE', #2027 ) ;
#16710 = DIRECTION ( 'NONE',  ( -0.2306359803922028717, -0.9730401042858035643, 4.849856555169146878E-15 ) ) ;
#16711 = DATE_AND_TIME ( #20296, #19820 ) ;
#16712 = CIRCLE ( 'NONE', #19762, 2.499999999999998224 ) ;
#16713 = ADVANCED_BREP_SHAPE_REPRESENTATION ( '', ( #9848, #12739 ), #5684 ) ;
#16714 = DATE_AND_TIME ( #13411, #17112 ) ;
#16715 =( BOUNDED_CURVE ( )  B_SPLINE_CURVE ( 2, ( #16497, #20423, #7488 ),
 .UNSPECIFIED., .F., .F. ) 
 B_SPLINE_CURVE_WITH_KNOTS ( ( 3, 3 ),
 ( 0.2928548593876180162, 0.5857097187752360323 ),
 .UNSPECIFIED. ) 
 CURVE ( )  GEOMETRIC_REPRESENTATION_ITEM ( )  RATIONAL_B_SPLINE_CURVE ( ( 1.000000000000000000, 1.037954849302039850, 1.000000000000000000 ) ) 
 REPRESENTATION_ITEM ( '' )  );
#16716 = DIRECTION ( 'NONE',  ( 0.9730401042858035643, -0.2306359803922028717, -5.958148513035547083E-17 ) ) ;
#16717 = LOCAL_TIME ( 14, 11, 27.00000000000000000, #22171 ) ;
#16718 = CC_DESIGN_SECURITY_CLASSIFICATION ( #12933, ( #14461 ) ) ;
#16719 = DIRECTION ( 'NONE',  ( -3.332946295912376778E-07, 0.000000000000000000, 0.9999999999999444888 ) ) ;
#16720 = CALENDAR_DATE ( 2026, 31, 10 ) ;
#16721 = ORGANIZATION ( 'NAUO-ORG38', 'UNSPECIFIED', 'UNSPECIFIED' ) ;
#16722 = VERTEX_POINT ( 'NONE', #9274 ) ;
#16723 = AXIS2_PLACEMENT_3D ( 'NONE', #506, #9679, #7760 ) ;
#16724 = DIRECTION ( 'NONE',  ( 0.0007613694435018767380, -0.9999997101582432935, 0.000000000000000000 ) ) ;
#16725 = ORIENTED_EDGE ( 'NONE', *, *, #4125, .F. ) ;
#16726 = EDGE_CURVE ( 'NONE', #20922, #18242, #14722, .T. ) ;
#16727 = CARTESIAN_POINT ( 'NONE',  ( 49.97703550743810297, 19.72589006657999988, -13.00000000000049916 ) ) ;
#16728 = CARTESIAN_POINT ( 'NONE',  ( 1.129445499342539821E-13, -1.843604948991550162E-16, -2.500000000000090150 ) ) ;
#16729 = DIRECTION ( 'NONE',  ( 0.7071067811865476838, -1.387778780781444689E-15, 0.7071067811865473507 ) ) ;
#16730 = ORIENTED_EDGE ( 'NONE', *, *, #18858, .F. ) ;
#16731 = ORIENTED_EDGE ( 'NONE', *, *, #4840, .T. ) ;
#16732 = CYLINDRICAL_SURFACE ( 'NONE', #1497, 4.349999999999996980 ) ;
#16733 = ORIENTED_EDGE ( 'NONE', *, *, #792, .T. ) ;
#16734 = CC_DESIGN_DATE_AND_TIME_ASSIGNMENT ( #9107, #4467, ( #16748 ) ) ;
#16735 = APPROVAL_DATE_TIME ( #2251, #10430 ) ;
#16736 = APPROVAL_PERSON_ORGANIZATION ( #14267, #16184, #5135 ) ;
#16737 = EDGE_LOOP ( 'NONE', ( #6689, #14209, #1373, #19925, #16554, #7498 ) ) ;
#16738 = ORIENTED_EDGE ( 'NONE', *, *, #10517, .F. ) ;
#16739 = DIRECTION ( 'NONE',  ( 0.2306359803922020946, 0.9730401042858036753, -4.006172263299086280E-15 ) ) ;
#16740 = CARTESIAN_POINT ( 'NONE',  ( -19.99999999999999645, -15.00000000000000000, 5.000000000004549250 ) ) ;
#16741 = COORDINATED_UNIVERSAL_TIME_OFFSET ( 0, 0, .AHEAD. ) ;
#16742 = CIRCLE ( 'NONE', #18271, 2.499999999999998668 ) ;
#16743 = EDGE_CURVE ( 'NONE', #12984, #21097, #1249, .T. ) ;
#16744 = DIRECTION ( 'NONE',  ( 0.000000000000000000, 1.020425574104004122E-16, 1.000000000000000000 ) ) ;
#16745 = EDGE_CURVE ( 'NONE', #12382, #4733, #13016, .T. ) ;
#16746 = AXIS2_PLACEMENT_3D ( 'NONE', #9401, #230, #14732 ) ;
#16747 = DIRECTION ( 'NONE',  ( -0.1630842657209349289, -0.6880432561069608211, -0.7071067811865437980 ) ) ;
#16748 = SECURITY_CLASSIFICATION ( '', '', #14574 ) ;
#16749 =( LENGTH_UNIT ( ) NAMED_UNIT ( * ) SI_UNIT ( .MILLI., .METRE. ) );
#16750 = ORIENTED_EDGE ( 'NONE', *, *, #14402, .F. ) ;
#16751 = DIRECTION ( 'NONE',  ( 1.000000000000000000, -4.028143194477080210E-16, -1.401298464324815982E-46 ) ) ;
#16752 = PERSON_AND_ORGANIZATION ( #11966, #8758 ) ;
#16753 = CC_DESIGN_APPROVAL ( #12713, ( #15459 ) ) ;
#16754 = ORIENTED_EDGE ( 'NONE', *, *, #19162, .F. ) ;
#16755 = DIRECTION ( 'NONE',  ( 0.005235963827117092427, -0.9999862922474493931, -2.636227439667000721E-16 ) ) ;
#16756 = LINE ( 'NONE', #20331, #1392 ) ;
#16757 = ORIENTED_EDGE ( 'NONE', *, *, #3297, .T. ) ;
#16758 = AXIS2_PLACEMENT_3D ( 'NONE', #431, #1992, #13162 ) ;
#16759 = ADVANCED_FACE ( 'NONE', ( #13531 ), #22660, .T. ) ;
#16760 = CYLINDRICAL_SURFACE ( 'NONE', #1773, 12.49999999999999645 ) ;
#16761 = AXIS2_PLACEMENT_3D ( 'NONE', #7817, #16587, #23395 ) ;
#16762 = CIRCLE ( 'NONE', #9609, 2.999999999999994227 ) ;
#16763 = DIRECTION ( 'NONE',  ( 0.000000000000000000, 0.000000000000000000, -1.000000000000000000 ) ) ;
#16764 = ORIENTED_EDGE ( 'NONE', *, *, #13892, .F. ) ;
#16765 = LOCAL_TIME ( 14, 11, 27.00000000000000000, #1864 ) ;
#16766 = DIRECTION ( 'NONE',  ( 0.2306359803922095053, 0.9730401042858018990, 0.000000000000000000 ) ) ;
#16767 = PRODUCT_RELATED_PRODUCT_CATEGORY ( 'detail', '', ( #14605 ) ) ;
#16768 = CIRCLE ( 'NONE', #22837, 2.499999999999999112 ) ;
#16769 = APPROVAL_ROLE ( '' ) ;
#16770 = ORIENTED_EDGE ( 'NONE', *, *, #22829, .T. ) ;
#16771 = PRODUCT_DEFINITION ( 'UNKNOWN', '', #19398, #7317 ) ;
#16772 = ORIENTED_EDGE ( 'NONE', *, *, #16086, .F. ) ;
#16773 = DIRECTION ( 'NONE',  ( -0.07397971354964408275, -0.9972597464969258363, 2.255140518769849223E-15 ) ) ;
#16774 = AXIS2_PLACEMENT_3D ( 'NONE', #15903, #1173, #17456 ) ;
#16775 = FACE_OUTER_BOUND ( 'NONE', #12857, .T. ) ;
#16776 = EDGE_LOOP ( 'NONE', ( #2490, #2216, #8813, #20036 ) ) ;
#16777 = PERSON_AND_ORGANIZATION_ROLE ( 'creator' ) ;
#16778 = ADVANCED_FACE ( 'NONE', ( #4505 ), #4627, .F. ) ;
#16779 = PLANE ( 'NONE',  #6966 ) ;
#16780 = ADVANCED_FACE ( 'NONE', ( #15422 ), #9999, .F. ) ;
#16781 = CC_DESIGN_SECURITY_CLASSIFICATION ( #8452, ( #6911 ) ) ;
#16782 = CC_DESIGN_PERSON_AND_ORGANIZATION_ASSIGNMENT ( #6320, #609, ( #14812 ) ) ;
#16783 = DIRECTION ( 'NONE',  ( 1.000000000000000000, -3.416070845000479880E-16, 0.000000000000000000 ) ) ;
#16784 = SECURITY_CLASSIFICATION_LEVEL ( 'unclassified' ) ;
#16785 = VECTOR ( 'NONE', #19032, 1000.000000000000000 ) ;
#16786 = DIRECTION ( 'NONE',  ( 0.2306359803922085339, 0.9730401042858022320, 0.000000000000000000 ) ) ;
#16787 = AXIS2_PLACEMENT_3D ( 'NONE', #9812, #8147, #20718 ) ;
#16788 = CIRCLE ( 'NONE', #17167, 0.3999999999999982458 ) ;
#16789 = CARTESIAN_POINT ( 'NONE',  ( 36.09092202081949807, 8.115512906978191054, -27.69000000000049866 ) ) ;
#16790 = AXIS2_PLACEMENT_3D ( 'NONE', #6598, #5149, #10167 ) ;
#16791 = CARTESIAN_POINT ( 'NONE',  ( -20.00000000000000000, -20.00000000000000000, 4.543842380125470691E-12 ) ) ;
#16792 = PERSON_AND_ORGANIZATION_ROLE ( 'creator' ) ;
#16793 = CARTESIAN_POINT ( 'NONE',  ( 0.000000000000000000, 2.220446049250309925E-15, -2.500000000000000000 ) ) ;
#16794 = VECTOR ( 'NONE', #23082, 999.9999999999998863 ) ;
#16795 = DIRECTION ( 'NONE',  ( 0.000000000000000000, -2.442084539047825566E-15, -1.000000000000000000 ) ) ;
#16796 = AXIS2_PLACEMENT_3D ( 'NONE', #19833, #20054, #14713 ) ;
#16797 = CARTESIAN_POINT ( 'NONE',  ( 34.50315935367051878, 10.80419468673749606, 27.44000000000020378 ) ) ;
#16798 = EDGE_CURVE ( 'NONE', #22224, #11059, #2957, .T. ) ;
#16799 = CC_DESIGN_APPROVAL ( #14736, ( #480 ) ) ;
#16800 = FACE_OUTER_BOUND ( 'NONE', #5835, .T. ) ;
#16801 = CARTESIAN_POINT ( 'NONE',  ( -68.02328523594360377, 12.24750435041217678, 3.945517663836197344E-15 ) ) ;
#16802 = AXIS2_PLACEMENT_3D ( 'NONE', #4035, #9644, #2494 ) ;
#16803 = DIRECTION ( 'NONE',  ( -0.005235963827108352890, 0.9999862922474493931, 5.936218956694023463E-19 ) ) ;
#16804 = VECTOR ( 'NONE', #19759, 1000.000000000000000 ) ;
#16805 = VERTEX_POINT ( 'NONE', #17231 ) ;
#16806 = TOROIDAL_SURFACE ( 'NONE', #18731, 3.750000000000000000, 0.5000000000000000000 ) ;
#16807 = ORIENTED_EDGE ( 'NONE', *, *, #20158, .T. ) ;
#16808 = DIRECTION ( 'NONE',  ( -0.9730401042858022320, 0.2306359803922080343, 5.959266323858941219E-17 ) ) ;
#16809 = DIRECTION ( 'NONE',  ( 0.000000000000000000, -2.442072289818050260E-15, -1.000000000000000000 ) ) ;
#16810 = ORIENTED_EDGE ( 'NONE', *, *, #17194, .F. ) ;
#16811 = ADVANCED_FACE ( 'NONE', ( #811, #15786 ), #15673, .T. ) ;
#16812 = DIRECTION ( 'NONE',  ( 1.164423685541410132E-14, 4.938475812832940103E-14, -1.000000000000000000 ) ) ;
#16813 = ORIENTED_EDGE ( 'NONE', *, *, #15306, .F. ) ;
#16814 = EDGE_CURVE ( 'NONE', #22303, #7126, #4976, .T. ) ;
#16815 = CARTESIAN_POINT ( 'NONE',  ( 106.2939232160746883, -18.21879530321555052, 13.00000000000000000 ) ) ;
#16816 = VECTOR ( 'NONE', #21892, 1000.000000000000114 ) ;
#16817 = APPROVAL_DATE_TIME ( #9337, #2413 ) ;
#16818 = CARTESIAN_POINT ( 'NONE',  ( 36.90212305349054844, 8.168604748878864896, -8.911899047890418757 ) ) ;
#16819 = ORGANIZATION ( 'NAUO-ORG5', 'UNSPECIFIED', 'UNSPECIFIED' ) ;
#16820 = AXIS2_PLACEMENT_3D ( 'NONE', #12113, #19334, #19686 ) ;
#16821 = ITEM_DEFINED_TRANSFORMATION ( 'NONE', 'NONE', #16146,  #12739 ) ;
#16822 = CIRCLE ( 'NONE', #18344, 0.3999999999999982458 ) ;
#16823 = PLANE ( 'NONE',  #23056 ) ;
#16824 = ORIENTED_EDGE ( 'NONE', *, *, #17411, .F. ) ;
#16825 = VECTOR ( 'NONE', #20745, 1000.000000000000227 ) ;
#16826 = DIRECTION ( 'NONE',  ( -0.04564792618501069266, -0.9989575901083128651, 2.775557561562892534E-15 ) ) ;
#16827 = EDGE_LOOP ( 'NONE', ( #11633, #14964, #21429, #6965, #21140, #7297, #5573, #1642, #1661, #4012, #438 ) ) ;
#16828 = DIRECTION ( 'NONE',  ( -0.9730401042858035643, 0.2306359803922028717, 5.958148513035547083E-17 ) ) ;
#16829 = DIRECTION ( 'NONE',  ( -0.9730401042858022320, 0.2306359803922080343, 5.959266323858941219E-17 ) ) ;
#16830 = EDGE_LOOP ( 'NONE', ( #20382, #17925, #23311, #6131 ) ) ;
#16831 = DIRECTION ( 'NONE',  ( 8.673617379884035472E-16, -1.000000000000000000, 0.000000000000000000 ) ) ;
#16832 = CARTESIAN_POINT ( 'NONE',  ( 1.836479826415680084E-19, -7.772252928343919938E-16, -8.889558542813568797E-14 ) ) ;
#16833 = ORIENTED_EDGE ( 'NONE', *, *, #22895, .F. ) ;
#16834 = VECTOR ( 'NONE', #6341, 999.9999999999998863 ) ;
#16835 = DATE_TIME_ROLE ( 'classification_date' ) ;
#16836 = LINE ( 'NONE', #7814, #13800 ) ;
#16837 = EDGE_CURVE ( 'NONE', #6052, #8980, #14904, .T. ) ;
#16838 = AXIS2_PLACEMENT_3D ( 'NONE', #23384, #5347, #1428 ) ;
#16839 = ORIENTED_EDGE ( 'NONE', *, *, #5400, .T. ) ;
#16840 = EDGE_CURVE ( 'NONE', #21775, #5571, #13386, .T. ) ;
#16841 = APPROVAL_DATE_TIME ( #4374, #9379 ) ;
#16842 = FACE_OUTER_BOUND ( 'NONE', #10446, .T. ) ;
#16843 = VERTEX_POINT ( 'NONE', #4858 ) ;
#16844 = ORIENTED_EDGE ( 'NONE', *, *, #125, .T. ) ;
#16845 = FACE_BOUND ( 'NONE', #10073, .T. ) ;
#16846 = DATE_AND_TIME ( #13172, #23215 ) ;
#16847 = DATE_TIME_ROLE ( 'classification_date' ) ;
#16848 = CYLINDRICAL_SURFACE ( 'NONE', #22555, 2.499999999999997780 ) ;
#16849 = CARTESIAN_POINT ( 'NONE',  ( 0.000000000000000000, 0.000000000000000000, 0.000000000000000000 ) ) ;
#16850 = LINE ( 'NONE', #11888, #17178 ) ;
#16851 = PERSON_AND_ORGANIZATION ( #11966, #8758 ) ;
#16852 = ORIENTED_EDGE ( 'NONE', *, *, #20712, .T. ) ;
#16853 = DIRECTION ( 'NONE',  ( -0.9730401042858035643, 0.2306359803922028717, 5.958148513035547083E-17 ) ) ;
#16854 = ORIENTED_EDGE ( 'NONE', *, *, #6029, .T. ) ;
#16855 = DIRECTION ( 'NONE',  ( 0.9999862922474493931, 0.005235963827108502076, 0.000000000000000000 ) ) ;
#16856 = CARTESIAN_POINT ( 'NONE',  ( -26.75688440168130100, 6.359989102302520791, -2.500292893218799772 ) ) ;
#16857 = DIRECTION ( 'NONE',  ( 1.040345436475888435E-32, 1.169424102322700040E-16, 1.000000000000000000 ) ) ;
#16858 = ORIENTED_EDGE ( 'NONE', *, *, #20747, .F. ) ;
#16859 = ORIENTED_EDGE ( 'NONE', *, *, #9691, .T. ) ;
#16860 = DIRECTION ( 'NONE',  ( -0.2306359803922026497, -0.9730401042858035643, 0.000000000000000000 ) ) ;
#16861 = ORIENTED_EDGE ( 'NONE', *, *, #20521, .T. ) ;
#16862 = DATE_TIME_ROLE ( 'classification_date' ) ;
#16863 = VERTEX_POINT ( 'NONE', #10343 ) ;
#16864 = VERTEX_POINT ( 'NONE', #12011 ) ;
#16865 = DIRECTION ( 'NONE',  ( -0.2306359803922033436, -0.9730401042858034533, 0.000000000000000000 ) ) ;
#16866 = SHAPE_REPRESENTATION ( '1602p_c_20', ( #12739 ), #21837 ) ;
#16867 = CALENDAR_DATE ( 2026, 31, 10 ) ;
#16868 = DIRECTION ( 'NONE',  ( -6.662111519016958720E-09, 1.000000000000000000, -2.523234146875356491E-15 ) ) ;
#16869 = VECTOR ( 'NONE', #18072, 1000.000000000000000 ) ;
#16870 = DIRECTION ( 'NONE',  ( 0.000000000000000000, 0.000000000000000000, -1.000000000000000000 ) ) ;
#16871 = EDGE_CURVE ( 'NONE', #4802, #17965, #20589, .T. ) ;
#16872 = EDGE_CURVE ( 'NONE', #7533, #9579, #3534, .T. ) ;
#16873 = ORIENTED_EDGE ( 'NONE', *, *, #7182, .F. ) ;
#16874 = CARTESIAN_POINT ( 'NONE',  ( 117.1011158151309957, -12.73035498497280038, 20.00000000000000000 ) ) ;
#16875 = PERSON_AND_ORGANIZATION ( #11966, #8758 ) ;
#16876 = AXIS2_PLACEMENT_3D ( 'NONE', #21282, #17623, #18166 ) ;
#16877 = EDGE_LOOP ( 'NONE', ( #23013, #6648, #21637, #5764 ) ) ;
#16878 = CARTESIAN_POINT ( 'NONE',  ( 114.8178196092480050, -22.36345201740219935, -20.00000000000000000 ) ) ;
#16879 = CARTESIAN_POINT ( 'NONE',  ( -14.54830929633820169, -2.787889851644860251, 6.750000000004459544 ) ) ;
#16880 = EDGE_LOOP ( 'NONE', ( #5213, #10339, #8669, #10442 ) ) ;
#16881 = EDGE_CURVE ( 'NONE', #15962, #2620, #2849, .T. ) ;
#16882 = EDGE_CURVE ( 'NONE', #16163, #15133, #8085, .T. ) ;
#16883 = DIRECTION ( 'NONE',  ( -0.9730401042858024541, 0.2306359803922080898, 5.959266323858952312E-17 ) ) ;
#16884 = DIRECTION ( 'NONE',  ( -0.2306359803922038432, -0.9730401042858032312, 5.139921410301653163E-15 ) ) ;
#16885 = EDGE_LOOP ( 'NONE', ( #2033, #4070, #11029, #19514 ) ) ;
#16886 = PLANE ( 'NONE',  #3504 ) ;
#16887 = CALENDAR_DATE ( 2026, 31, 10 ) ;
#16888 = PRODUCT_DEFINITION_SHAPE ( 'NONE', 'NONE',  #13165 ) ;
#16889 = VERTEX_POINT ( 'NONE', #1164 ) ;
#16890 = ORIENTED_EDGE ( 'NONE', *, *, #22920, .T. ) ;
#16891 = FACE_OUTER_BOUND ( 'NONE', #1172, .T. ) ;
#16892 = DIRECTION ( 'NONE',  ( -2.982858504577314686E-17, 2.441916418604790135E-15, 1.000000000000000000 ) ) ;
#16893 =( REPRESENTATION_RELATIONSHIP ('NONE','NONE', #19303, #11141 ) REPRESENTATION_RELATIONSHIP_WITH_TRANSFORMATION ( #18026 )SHAPE_REPRESENTATION_RELATIONSHIP( ) );
#16894 = ORIENTED_EDGE ( 'NONE', *, *, #2518, .F. ) ;
#16895 = APPROVAL_ROLE ( '' ) ;
#16896 = CARTESIAN_POINT ( 'NONE',  ( -24.86147400983239919, -14.96352599016710094, -2.500000000000000000 ) ) ;
#16897 = AXIS2_PLACEMENT_3D ( 'NONE', #23348, #14575, #7106 ) ;
#16898 = PLANE ( 'NONE',  #22265 ) ;
#16899 = ITEM_DEFINED_TRANSFORMATION ( 'NONE', 'NONE', #6844,  #15386 ) ;
#16900 = FACE_OUTER_BOUND ( 'NONE', #14002, .T. ) ;
#16901 = AXIS2_PLACEMENT_3D ( 'NONE', #7544, #21658, #9086 ) ;
#16902 = EDGE_CURVE ( 'NONE', #928, #20160, #22547, .T. ) ;
#16903 = CARTESIAN_POINT ( 'NONE',  ( 60.98218416654080443, 14.99311160239464336, 13.00000000000000000 ) ) ;
#16904 = CC_DESIGN_DATE_AND_TIME_ASSIGNMENT ( #3372, #21534, ( #5445 ) ) ;
#16905 = LINE ( 'NONE', #5746, #5982 ) ;
#16906 = SHAPE_DEFINITION_REPRESENTATION ( #8719, #18771 ) ;
#16907 = PRODUCT_DEFINITION ( 'UNKNOWN', '', #3492, #12095 ) ;
#16908 = PLANE ( 'NONE',  #14569 ) ;
#16909 = DIRECTION ( 'NONE',  ( -0.9730401042858036753, 0.2306359803922028995, 5.958148513035547083E-17 ) ) ;
#16910 = EDGE_CURVE ( 'NONE', #12727, #11662, #16405, .T. ) ;
#16911 = ADVANCED_FACE ( 'NONE', ( #17803 ), #12582, .T. ) ;
#16912 = CARTESIAN_POINT ( 'NONE',  ( 118.4388045014059969, -7.086722380115130449, 18.89999999999999858 ) ) ;
#16913 = LINE ( 'NONE', #18939, #10308 ) ;
#16914 = DIRECTION ( 'NONE',  ( -6.123230199561459225E-17, -4.868008300101910084E-15, -1.000000000000000000 ) ) ;
#16915 = CARTESIAN_POINT ( 'NONE',  ( 117.0319250210129951, -13.02226701625859917, 15.90000000000000036 ) ) ;
#16916 = ORIENTED_EDGE ( 'NONE', *, *, #8037, .T. ) ;
#16917 = AXIS2_PLACEMENT_3D ( 'NONE', #19016, #11918, #7852 ) ;
#16918 = EDGE_LOOP ( 'NONE', ( #3215, #14609, #3756, #5344 ) ) ;
#16919 = DIRECTION ( 'NONE',  ( 5.401314170743249993E-15, 2.304622183485879988E-14, -1.000000000000000000 ) ) ;
#16920 = CARTESIAN_POINT ( 'NONE',  ( 28.89837840081079889, -1.998294948772295410, -8.750000000000399680 ) ) ;
#16921 = ORIENTED_EDGE ( 'NONE', *, *, #1441, .T. ) ;
#16922 = CARTESIAN_POINT ( 'NONE',  ( 5.000000000000000000, -31.09999999999999787, 21.50000000000000000 ) ) ;
#16923 = VERTEX_POINT ( 'NONE', #16012 ) ;
#16924 = DIRECTION ( 'NONE',  ( 0.000000000000000000, 0.000000000000000000, 1.000000000000000000 ) ) ;
#16925 = SHAPE_DEFINITION_REPRESENTATION ( #20305, #4731 ) ;
#16926 = CARTESIAN_POINT ( 'NONE',  ( 37.48433000560739714, 10.62229491794307279, -8.912006346179977001 ) ) ;
#16927 = EDGE_CURVE ( 'NONE', #12098, #16935, #4678, .T. ) ;
#16928 = AXIS2_PLACEMENT_3D ( 'NONE', #18188, #12844, #19737 ) ;
#16929 = PERSON_AND_ORGANIZATION ( #3121, #3112 ) ;
#16930 = AXIS2_PLACEMENT_3D ( 'NONE', #20091, #19749, #19982 ) ;
#16931 =( LENGTH_UNIT ( ) NAMED_UNIT ( * ) SI_UNIT ( .MILLI., .METRE. ) );
#16932 = DIRECTION ( 'NONE',  ( 0.9999862922474492821, 0.005235963827109980928, 0.000000000000000000 ) ) ;
#16933 = ORIENTED_EDGE ( 'NONE', *, *, #289, .T. ) ;
#16934 = CARTESIAN_POINT ( 'NONE',  ( 43.84419854219520829, 0.000000000000000000, 25.00000000000000000 ) ) ;
#16935 = VERTEX_POINT ( 'NONE', #12700 ) ;
#16936 = CARTESIAN_POINT ( 'NONE',  ( 33.87671241911665021, -0.5062525893941096644, -13.00000000000039968 ) ) ;
#16937 = EDGE_CURVE ( 'NONE', #3635, #9993, #23362, .T. ) ;
#16938 = EDGE_CURVE ( 'NONE', #17080, #16923, #19696, .T. ) ;
#16939 = MANIFOLD_SOLID_BREP ( 'Imported1', #11363 ) ;
#16940 = CARTESIAN_POINT ( 'NONE',  ( 118.5310588935630136, -6.697506338400819992, 20.00000000000000000 ) ) ;
#16941 = ORIENTED_EDGE ( 'NONE', *, *, #1963, .T. ) ;
#16942 = CARTESIAN_POINT ( 'NONE',  ( 43.84419854219520829, -31.09999999999999787, -21.49999999999999645 ) ) ;
#16943 = DIRECTION ( 'NONE',  ( 0.000000000000000000, -1.000000000000000000, 1.998401444326210262E-15 ) ) ;
#16944 = ORIENTED_EDGE ( 'NONE', *, *, #6936, .T. ) ;
#16945 = CIRCLE ( 'NONE', #9373, 2.500000000000000000 ) ;
#16946 = CALENDAR_DATE ( 2026, 31, 10 ) ;
#16947 = VECTOR ( 'NONE', #19127, 1000.000000000000000 ) ;
#16948 = CARTESIAN_POINT ( 'NONE',  ( 36.17078849317572775, 12.20740994216800601, 17.69999999999998863 ) ) ;
#16949 = VECTOR ( 'NONE', #12400, 1000.000000000000227 ) ;
#16950 = ORIENTED_EDGE ( 'NONE', *, *, #4857, .T. ) ;
#16951 = PERSON_AND_ORGANIZATION_ROLE ( 'creator' ) ;
#16952 = CARTESIAN_POINT ( 'NONE',  ( -26.00000000000209610, -20.00000000055539928, -7.999999999994108713 ) ) ;
#16953 = VERTEX_POINT ( 'NONE', #23120 ) ;
#16954 = ORIENTED_EDGE ( 'NONE', *, *, #4009, .F. ) ;
#16955 = DIRECTION ( 'NONE',  ( 2.269747459788990007E-13, 2.220446049250330436E-15, 1.000000000000000000 ) ) ;
#16956 = MECHANICAL_CONTEXT ( 'NONE', #7024, 'mechanical' ) ;
#16957 = EDGE_CURVE ( 'NONE', #7019, #5544, #17923, .T. ) ;
#16958 = CONTEXT_DEPENDENT_SHAPE_REPRESENTATION ( #14924, #9899 ) ;
#16959 = CIRCLE ( 'NONE', #21131, 7.000000000000000888 ) ;
#16960 = LINE ( 'NONE', #14952, #15359 ) ;
#16961 = EDGE_CURVE ( 'NONE', #3332, #8528, #14235, .T. ) ;
#16962 = CIRCLE ( 'NONE', #12437, 2.379999999999999893 ) ;
#16963 = AXIS2_PLACEMENT_3D ( 'NONE', #4766, #18912, #6791 ) ;
#16964 = CARTESIAN_POINT ( 'NONE',  ( 34.24699604337060066, 12.59578995394270073, 5.000000000000000000 ) ) ;
#16965 = VERTEX_POINT ( 'NONE', #10694 ) ;
#16966 = EDGE_CURVE ( 'NONE', #6033, #171, #17183, .T. ) ;
#16967 = APPROVAL_DATE_TIME ( #4271, #17811 ) ;
#16968 = EDGE_CURVE ( 'NONE', #13084, #19582, #3419, .T. ) ;
#16969 = EDGE_LOOP ( 'NONE', ( #17373, #5325, #16461, #13909 ) ) ;
#16970 = CARTESIAN_POINT ( 'NONE',  ( -31.64160538070510142, 6.334412527122569969, -5.000000000000000000 ) ) ;
#16971 = EDGE_LOOP ( 'NONE', ( #18532, #22158 ) ) ;
#16972 = CARTESIAN_POINT ( 'NONE',  ( -20.00000002062810367, 25.45208919256889857, 4.448570609349010398E-12 ) ) ;
#16973 = CARTESIAN_POINT ( 'NONE',  ( -58.60882321939761397, 12.73364205572179841, 2.500000000000008882 ) ) ;
#16974 = PLANE ( 'NONE',  #20607 ) ;
#16975 = CIRCLE ( 'NONE', #16215, 2.066999999999999726 ) ;
#16976 = ORIENTED_EDGE ( 'NONE', *, *, #4410, .T. ) ;
#16977 = VERTEX_POINT ( 'NONE', #21473 ) ;
#16978 = DIRECTION ( 'NONE',  ( -0.9730401042858036753, 0.2306359803922028995, -2.804983810440358801E-16 ) ) ;
#16979 = ORIENTED_EDGE ( 'NONE', *, *, #15162, .F. ) ;
#16980 = PERSON_AND_ORGANIZATION_ROLE ( 'classification_officer' ) ;
#16981 = AXIS2_PLACEMENT_3D ( 'NONE', #5521, #161, #16211 ) ;
#16982 = MANIFOLD_SOLID_BREP ( 'Imported1', #12484 ) ;
#16983 = VERTEX_POINT ( 'NONE', #5447 ) ;
#16984 = ORIENTED_EDGE ( 'NONE', *, *, #11287, .T. ) ;
#16985 = DIRECTION ( 'NONE',  ( -0.9730401042858022320, 0.2306359803922080343, 5.959266323858941219E-17 ) ) ;
#16986 = VECTOR ( 'NONE', #12768, 999.9999999999998863 ) ;
#16987 = CALENDAR_DATE ( 2026, 31, 10 ) ;
#16988 = DIRECTION ( 'NONE',  ( -2.269747459788994803E-13, -2.220446049250325308E-15, -1.000000000000000000 ) ) ;
#16989 = CARTESIAN_POINT ( 'NONE',  ( 35.59419854219520118, 9.774809681453278998, -27.87500000000050093 ) ) ;
#16990 = CIRCLE ( 'NONE', #11328, 7.000000000000000000 ) ;
#16991 = APPROVAL ( #18195, 'UNSPECIFIED' ) ;
#16992 =( NAMED_UNIT ( * ) SI_UNIT ( $, .STERADIAN. ) SOLID_ANGLE_UNIT ( ) );
#16993 = CIRCLE ( 'NONE', #4859, 2.650000000000001688 ) ;
#16994 = DIRECTION ( 'NONE',  ( 0.000000000000000000, 0.000000000000000000, 1.000000000000000000 ) ) ;
#16995 = PERSON_AND_ORGANIZATION ( #11966, #8758 ) ;
#16996 = CONICAL_SURFACE ( 'NONE', #23058, 5.086751345948125724, 1.047197551196598297 ) ;
#16997 = ORIENTED_EDGE ( 'NONE', *, *, #16315, .F. ) ;
#16998 = PLANE ( 'NONE',  #6074 ) ;
#16999 = DIRECTION ( 'NONE',  ( -0.9730401042858022320, 0.2306359803922080343, 5.959266323858941219E-17 ) ) ;
#17000 = PERSON ( 'NAUO-PER27', 'UNSPECIFIED', 'UNSPECIFIED', ('UNSPECIFIED'), ('UNSPECIFIED'), ('UNSPECIFIED') ) ;
#17001 = ORIENTED_EDGE ( 'NONE', *, *, #20735, .T. ) ;
#17002 = DIRECTION ( 'NONE',  ( -0.9730401042858022320, 0.2306359803922080343, 5.959266323858941219E-17 ) ) ;
#17003 = CARTESIAN_POINT ( 'NONE',  ( 122.4288069621910040, 9.746871424029281528, -13.00000000000000000 ) ) ;
#17004 = ORIENTED_EDGE ( 'NONE', *, *, #15435, .F. ) ;
#17005 = CARTESIAN_POINT ( 'NONE',  ( 36.36149123738979938, 11.13450152885909894, 29.25000000000000000 ) ) ;
#17006 = PERSON_AND_ORGANIZATION_ROLE ( 'design_owner' ) ;
#17007 = EDGE_CURVE ( 'NONE', #6789, #3813, #11905, .T. ) ;
#17008 = VERTEX_POINT ( 'NONE', #9014 ) ;
#17009 = VERTEX_POINT ( 'NONE', #1512 ) ;
#17010 = CARTESIAN_POINT ( 'NONE',  ( 29.35071467092108577, -7.244044837847749108, 13.00000000000000000 ) ) ;
#17011 = CARTESIAN_POINT ( 'NONE',  ( -27.50000000434249969, 26.95208919188020147, 5.500000000004539480 ) ) ;
#17012 = FACE_OUTER_BOUND ( 'NONE', #16421, .T. ) ;
#17013 = APPLICATION_PROTOCOL_DEFINITION ( 'international standard', 'config_control_design', 1994, #608 ) ;
#17014 = CARTESIAN_POINT ( 'NONE',  ( -19.99999998168114601, -22.75000000000000000, -8.499999999995452526 ) ) ;
#17015 = CARTESIAN_POINT ( 'NONE',  ( 34.89491389100810181, 23.30074776265909975, -13.00000000000049916 ) ) ;
#17016 = AXIS2_PLACEMENT_3D ( 'NONE', #3757, #16464, #10681 ) ;
#17017 = PERSON_AND_ORGANIZATION_ROLE ( 'classification_officer' ) ;
#17018 = CARTESIAN_POINT ( 'NONE',  ( -20.00000000397270128, 22.95208919257349933, 8.000000000004460432 ) ) ;
#17019 = MANIFOLD_SOLID_BREP ( 'Imported1', #13610 ) ;
#17020 = DIRECTION ( 'NONE',  ( -0.9730401042858021210, 0.2306359803922091167, -1.531342102931250897E-15 ) ) ;
#17021 = DIRECTION ( 'NONE',  ( -0.9997648975362222190, -0.02168293463503410262, 0.000000000000000000 ) ) ;
#17022 = DATE_AND_TIME ( #22237, #3068 ) ;
#17023 = FACE_OUTER_BOUND ( 'NONE', #17553, .T. ) ;
#17024 = CARTESIAN_POINT ( 'NONE',  ( 82.99337969622625621, -17.64642043817435990, -13.00000000000000000 ) ) ;
#17025 = DIRECTION ( 'NONE',  ( 1.751019220569994795E-16, 2.300154215587015208E-15, 1.000000000000000000 ) ) ;
#17026 = CARTESIAN_POINT ( 'NONE',  ( 39.27359436029389883, 22.26288585089444894, 12.99999999999979927 ) ) ;
#17027 = DIRECTION ( 'NONE',  ( -0.9997648975362221080, -0.02168293463503390486, 0.000000000000000000 ) ) ;
#17028 = ORIENTED_EDGE ( 'NONE', *, *, #7027, .F. ) ;
#17029 = EDGE_CURVE ( 'NONE', #22086, #11012, #2397, .T. ) ;
#17030 = VERTEX_POINT ( 'NONE', #16129 ) ;
#17031 = CARTESIAN_POINT ( 'NONE',  ( -14.70588235717629821, 25.77561860482770228, -5.499999999996769695 ) ) ;
#17032 = DIRECTION ( 'NONE',  ( 0.000000000000000000, 0.000000000000000000, 1.000000000000000000 ) ) ;
#17033 = COORDINATED_UNIVERSAL_TIME_OFFSET ( 0, 0, .AHEAD. ) ;
#17034 = ORIENTED_EDGE ( 'NONE', *, *, #5598, .F. ) ;
#17035 = CIRCLE ( 'NONE', #8329, 49.22658835543909817 ) ;
#17036 = CC_DESIGN_PERSON_AND_ORGANIZATION_ASSIGNMENT ( #17323, #4841, ( #8779 ) ) ;
#17037 = CARTESIAN_POINT ( 'NONE',  ( 37.37362508103680625, 25.08661566644159890, 13.00000000000000000 ) ) ;
#17038 = ORIENTED_EDGE ( 'NONE', *, *, #10005, .F. ) ;
#17039 = DIRECTION ( 'NONE',  ( 0.9730401042858024541, -0.2306359803922080898, -5.959266323858942451E-17 ) ) ;
#17040 = PERSON_AND_ORGANIZATION ( #11966, #8758 ) ;
#17041 = DIRECTION ( 'NONE',  ( 5.964507377817269296E-17, 4.861311874385510251E-15, 1.000000000000000000 ) ) ;
#17042 = EDGE_CURVE ( 'NONE', #21488, #16923, #7123, .T. ) ;
#17043 = EDGE_CURVE ( 'NONE', #23363, #5959, #19933, .T. ) ;
#17044 = COORDINATED_UNIVERSAL_TIME_OFFSET ( 0, 0, .AHEAD. ) ;
#17045 =( NAMED_UNIT ( * ) SI_UNIT ( $, .STERADIAN. ) SOLID_ANGLE_UNIT ( ) );
#17046 = DIRECTION ( 'NONE',  ( -0.9730401042858036753, 0.2306359803922031493, -2.804983810440361760E-16 ) ) ;
#17047 = EDGE_CURVE ( 'NONE', #15102, #2850, #3551, .T. ) ;
#17048 = AXIS2_PLACEMENT_3D ( 'NONE', #16068, #8707, #6811 ) ;
#17049 = CARTESIAN_POINT ( 'NONE',  ( 34.49867763533220710, 5.152869186095990983, 27.87500000000002487 ) ) ;
#17050 = ORIENTED_EDGE ( 'NONE', *, *, #12325, .T. ) ;
#17051 = DIRECTION ( 'NONE',  ( -0.8511275218278966381, -0.5249589903860140128, 5.212440122911323074E-17 ) ) ;
#17052 = MANIFOLD_SOLID_BREP ( 'Boss-Extrude4', #9913 ) ;
#17053 = CARTESIAN_POINT ( 'NONE',  ( 43.98050001724080005, -5.573152644851309567, 13.00000000000019895 ) ) ;
#17054 = ORIENTED_EDGE ( 'NONE', *, *, #15947, .F. ) ;
#17055 = VECTOR ( 'NONE', #18011, 999.9999999999998863 ) ;
#17056 = DIRECTION ( 'NONE',  ( -0.2306359803922102825, -0.9730401042858017879, 4.163336342344335449E-15 ) ) ;
#17057 = LINE ( 'NONE', #15283, #8775 ) ;
#17058 = ORIENTED_EDGE ( 'NONE', *, *, #10006, .T. ) ;
#17059 = EDGE_CURVE ( 'NONE', #21956, #8342, #20235, .T. ) ;
#17060 = CARTESIAN_POINT ( 'NONE',  ( -23.50000000000000000, -20.00000000000000000, 0.000000000000000000 ) ) ;
#17061 = ORIENTED_EDGE ( 'NONE', *, *, #16910, .F. ) ;
#17063 = APPROVAL_ROLE ( '' ) ;
#17062 = PRODUCT_DEFINITION ( 'UNKNOWN', '', #15652, #22978 ) ;
#17064 = DIRECTION ( 'NONE',  ( 1.224646799147353207E-16, 1.000000000000000000, -0.000000000000000000 ) ) ;
#17065 = VERTEX_POINT ( 'NONE', #5409 ) ;
#17066 = APPROVAL_PERSON_ORGANIZATION ( #18649, #659, #14955 ) ;
#17067 = EDGE_LOOP ( 'NONE', ( #9310, #4484 ) ) ;
#17068 = APPROVAL ( #21238, 'UNSPECIFIED' ) ;
#17069 = AXIS2_PLACEMENT_3D ( 'NONE', #8623, #12205, #23084 ) ;
#17070 = APPLICATION_PROTOCOL_DEFINITION ( 'international standard', 'config_control_design', 1994, #7024 ) ;
#17071 = CIRCLE ( 'NONE', #20108, 2.500000000000000888 ) ;
#17072 = EDGE_CURVE ( 'NONE', #13995, #5198, #22015, .T. ) ;
#17073 = EDGE_CURVE ( 'NONE', #23388, #6910, #22891, .T. ) ;
#17074 = CC_DESIGN_PERSON_AND_ORGANIZATION_ASSIGNMENT ( #15346, #11461, ( #14615 ) ) ;
#17075 = COORDINATED_UNIVERSAL_TIME_OFFSET ( 0, 0, .AHEAD. ) ;
#17076 = DIRECTION ( 'NONE',  ( 0.9730401042858035643, -0.2306359803922028717, -5.432877459303547053E-17 ) ) ;
#17077 = CONICAL_SURFACE ( 'NONE', #3792, 2.283499999999998753, 0.7853981633974433940 ) ;
#17078 = AXIS2_PLACEMENT_3D ( 'NONE', #7615, #3697, #16621 ) ;
#17079 = CARTESIAN_POINT ( 'NONE',  ( 43.98050001724070057, -5.573152644851429471, -13.00000000000039968 ) ) ;
#17080 = VERTEX_POINT ( 'NONE', #13014 ) ;
#17081 = APPROVAL_STATUS ( 'not_yet_approved' ) ;
#17082 = PRODUCT ( 'Fixed base', 'Fixed base', '', ( #10180 ) ) ;
#17083 = LOCAL_TIME ( 14, 11, 27.00000000000000000, #848 ) ;
#17084 = ORIENTED_EDGE ( 'NONE', *, *, #22601, .F. ) ;
#17085 = CC_DESIGN_APPROVAL ( #21194, ( #4231 ) ) ;
#17086 = CARTESIAN_POINT ( 'NONE',  ( 1.137438022745850001E-13, -8.410916347709809861E-16, 2.500000000000090150 ) ) ;
#17087 = DIRECTION ( 'NONE',  ( -0.9730401042858022320, 0.2306359803922080343, 5.959266323858941219E-17 ) ) ;
#17088 = ORIENTED_EDGE ( 'NONE', *, *, #3395, .F. ) ;
#17089 = ADVANCED_FACE ( 'NONE', ( #3513, #3855 ), #12672, .T. ) ;
#17090 = DIRECTION ( 'NONE',  ( -2.982858504577319616E-17, 2.441916418604790135E-15, 1.000000000000000000 ) ) ;
#17091 = FACE_OUTER_BOUND ( 'NONE', #20280, .T. ) ;
#17092 = DIRECTION ( 'NONE',  ( 0.005225493764075828107, -0.9999863470142589250, 2.602085213965210642E-15 ) ) ;
#17093 = ORIENTED_EDGE ( 'NONE', *, *, #3107, .F. ) ;
#17094 = ORIENTED_EDGE ( 'NONE', *, *, #22988, .T. ) ;
#17095 = DIRECTION ( 'NONE',  ( 0.005235963827108352890, -0.9999862922474493931, -5.936218956694023463E-19 ) ) ;
#17096 = EDGE_LOOP ( 'NONE', ( #9501, #20024 ) ) ;
#17097 = VECTOR ( 'NONE', #20632, 1000.000000000000000 ) ;
#17098 = DATE_AND_TIME ( #588, #1547 ) ;
#17099 = MANIFOLD_SOLID_BREP ( 'Imported1', #20812 ) ;
#17100 = EDGE_CURVE ( 'NONE', #4764, #21792, #11133, .T. ) ;
#17101 = EDGE_LOOP ( 'NONE', ( #5534, #4459, #2253, #11462 ) ) ;
#17102 = EDGE_LOOP ( 'NONE', ( #12012, #15683, #13525, #13436 ) ) ;
#17103 = LINE ( 'NONE', #22203, #12986 ) ;
#17104 = PERSON_AND_ORGANIZATION ( #11966, #8758 ) ;
#17105 = CLOSED_SHELL ( 'NONE', ( #10826, #12882, #6970, #17782, #6453, #18138, #1651, #2665, #9816, #20595, #5799, #18103, #18535, #22483, #3266, #16065, #10456, #3324, #6004, #17464, #20249, #5650, #13185, #3992, #49 ) ) ;
#17106 = ADVANCED_FACE ( 'NONE', ( #12777 ), #1721, .F. ) ;
#17107 = CC_DESIGN_APPROVAL ( #6196, ( #14070 ) ) ;
#17108 = EDGE_CURVE ( 'NONE', #11071, #3143, #21367, .T. ) ;
#17109 = CARTESIAN_POINT ( 'NONE',  ( 28.65327419723657343, 2.170628644843063615, -6.523238081173185874E-16 ) ) ;
#17110 = APPROVAL_PERSON_ORGANIZATION ( #9285, #12713, #21853 ) ;
#17111 = AXIS2_PLACEMENT_3D ( 'NONE', #17310, #15394, #11635 ) ;
#17112 = LOCAL_TIME ( 14, 11, 27.00000000000000000, #9742 ) ;
#17113 = AXIS2_PLACEMENT_3D ( 'NONE', #164, #7431, #7198 ) ;
#17114 = DIRECTION ( 'NONE',  ( -0.9730401042858024541, 0.2306359803922080898, 5.959266323858942451E-17 ) ) ;
#17115 = COORDINATED_UNIVERSAL_TIME_OFFSET ( 0, 0, .AHEAD. ) ;
#17116 = VERTEX_POINT ( 'NONE', #8981 ) ;
#17117 = CARTESIAN_POINT ( 'NONE',  ( 31.56827854690379098, -0.8510906712621758574, 12.00000000000019185 ) ) ;
#17118 = DIRECTION ( 'NONE',  ( 0.005235963827117092427, -0.9999862922474493931, -2.636227439667000721E-16 ) ) ;
#17119 = VERTEX_POINT ( 'NONE', #14560 ) ;
#17120 = LOCAL_TIME ( 14, 11, 27.00000000000000000, #8824 ) ;
#17121 = CYLINDRICAL_SURFACE ( 'NONE', #12056, 2.750000000000000000 ) ;
#17122 = CARTESIAN_POINT ( 'NONE',  ( -20.00000000000000000, -20.00000000000000000, -2.500000000000000000 ) ) ;
#17123 = LOCAL_TIME ( 14, 11, 27.00000000000000000, #10399 ) ;
#17124 = ORIENTED_EDGE ( 'NONE', *, *, #12556, .T. ) ;
#17125 = LINE ( 'NONE', #11342, #16009 ) ;
#17126 = AXIS2_PLACEMENT_3D ( 'NONE', #9991, #1156, #9859 ) ;
#17127 = APPROVAL_DATE_TIME ( #4185, #15337 ) ;
#17128 = VERTEX_POINT ( 'NONE', #7548 ) ;
#17129 = EDGE_LOOP ( 'NONE', ( #14155, #6436, #5889, #13250 ) ) ;
#17130 = FACE_BOUND ( 'NONE', #1390, .T. ) ;
#17131 = CARTESIAN_POINT ( 'NONE',  ( -19.49999999982360066, -0.1021026942259749964, -2.500000000000000000 ) ) ;
#17132 = CC_DESIGN_APPROVAL ( #14864, ( #7962 ) ) ;
#17133 = EDGE_LOOP ( 'NONE', ( #14562, #20402, #20981, #17609 ) ) ;
#17134 = SHAPE_DEFINITION_REPRESENTATION ( #23105, #16866 ) ;
#17135 = DIRECTION ( 'NONE',  ( 0.000000000000000000, -1.000000000000000000, 5.035481788031372371E-15 ) ) ;
#17136 = CARTESIAN_POINT ( 'NONE',  ( -20.36989857172092044, 17.96579046008427127, -4.999999999995548450 ) ) ;
#17137 = SECURITY_CLASSIFICATION_LEVEL ( 'unclassified' ) ;
#17138 = CARTESIAN_POINT ( 'NONE',  ( -25.01253141238790079, 26.70208918381559826, -5.499999999994429345 ) ) ;
#17139 = MANIFOLD_SOLID_BREP ( 'Boss-Extrude1', #1085 ) ;
#17140 = LOCAL_TIME ( 14, 11, 27.00000000000000000, #19356 ) ;
#17141 =( LENGTH_UNIT ( ) NAMED_UNIT ( * ) SI_UNIT ( .MILLI., .METRE. ) );
#17142 = AXIS2_PLACEMENT_3D ( 'NONE', #14936, #21814, #7351 ) ;
#17143 = EDGE_CURVE ( 'NONE', #23068, #8432, #18237, .T. ) ;
#17144 = CARTESIAN_POINT ( 'NONE',  ( 30.84445860938240003, -2.459566909556570202, 8.750000000000198952 ) ) ;
#17145 = DATE_TIME_ROLE ( 'classification_date' ) ;
#17146 = VECTOR ( 'NONE', #6635, 1000.000000000000227 ) ;
#17147 = AXIS2_PLACEMENT_3D ( 'NONE', #7782, #879, #13590 ) ;
#17148 = LOCAL_TIME ( 14, 11, 27.00000000000000000, #5550 ) ;
#17149 = FACE_BOUND ( 'NONE', #15454, .T. ) ;
#17150 = DIRECTION ( 'NONE',  ( -1.187319687680494078E-16, -2.805478249478265308E-20, -1.000000000000000000 ) ) ;
#17151 = VECTOR ( 'NONE', #14031, 1000.000000000000000 ) ;
#17152 = CARTESIAN_POINT ( 'NONE',  ( 33.27836309399498305, 10.32372331478672223, -26.88000000000050349 ) ) ;
#17153 = DIRECTION ( 'NONE',  ( -0.9999862922474491711, -0.005235963827128302210, 1.239088197126291310E-16 ) ) ;
#17154 = CONICAL_SURFACE ( 'NONE', #6992, 0.8660254037844397068, 1.047197551196598297 ) ;
#17155 = DIRECTION ( 'NONE',  ( 0.000000000000000000, 1.156482317317871478E-16, 1.000000000000000000 ) ) ;
#17156 = CARTESIAN_POINT ( 'NONE',  ( -17.47493720815189633, 28.95208920939580111, 8.000000000004419576 ) ) ;
#17157 = EDGE_LOOP ( 'NONE', ( #802, #2366, #6596, #3239 ) ) ;
#17158 = CC_DESIGN_APPROVAL ( #17381, ( #17062 ) ) ;
#17159 = ORIENTED_EDGE ( 'NONE', *, *, #2846, .T. ) ;
#17160 = DIRECTION ( 'NONE',  ( -0.1630842657209350399, -0.6880432561069612651, -0.7071067811865433539 ) ) ;
#17161 = DIRECTION ( 'NONE',  ( -0.2306359803922019835, -0.9730401042858037863, 4.163336342344336238E-15 ) ) ;
#17162 = ORIENTED_EDGE ( 'NONE', *, *, #5888, .F. ) ;
#17163 = CIRCLE ( 'NONE', #6554, 2.499999999999998668 ) ;
#17164 = CIRCLE ( 'NONE', #19073, 2.386550000000003724 ) ;
#17165 = DIRECTION ( 'NONE',  ( 1.013160721610911865E-47, -1.000000000000000000, 2.441916418604790135E-15 ) ) ;
#17166 = ORIENTED_EDGE ( 'NONE', *, *, #17800, .F. ) ;
#17167 = AXIS2_PLACEMENT_3D ( 'NONE', #10523, #4926, #12190 ) ;
#17168 = PLANE ( 'NONE',  #21597 ) ;
#17169 = PERSON_AND_ORGANIZATION ( #11966, #8758 ) ;
#17170 = CARTESIAN_POINT ( 'NONE',  ( 33.90884364377009774, 10.17428291754630010, 28.46999999999999886 ) ) ;
#17171 = APPLICATION_CONTEXT ( 'configuration controlled 3d designs of mechanical parts and assemblies' ) ;
#17172 = CIRCLE ( 'NONE', #2390, 4.999999999999995559 ) ;
#17173 = PERSON_AND_ORGANIZATION ( #14196, #4621 ) ;
#17174 = CARTESIAN_POINT ( 'NONE',  ( 0.000000000000000000, 0.000000000000000000, 0.000000000000000000 ) ) ;
#17175 = TOROIDAL_SURFACE ( 'NONE', #20213, 2.600000000000000089, 0.1000000000000000056 ) ;
#17176 = EDGE_CURVE ( 'NONE', #15056, #18433, #21789, .T. ) ;
#17178 = VECTOR ( 'NONE', #2362, 1000.000000000000000 ) ;
#17177 = FACE_OUTER_BOUND ( 'NONE', #9751, .T. ) ;
#17179 = EDGE_CURVE ( 'NONE', #8503, #2209, #17885, .T. ) ;
#17180 = DIRECTION ( 'NONE',  ( 5.039379565342698073E-16, -1.000000000000000000, 0.000000000000000000 ) ) ;
#17181 = LOCAL_TIME ( 14, 11, 27.00000000000000000, #7909 ) ;
#17182 = DIRECTION ( 'NONE',  ( 0.2306359803922080343, 0.9730401042858022320, 1.780177465867830349E-15 ) ) ;
#17183 = CIRCLE ( 'NONE', #22098, 0.3999999999999998557 ) ;
#17184 = EDGE_LOOP ( 'NONE', ( #8189, #20691, #14683, #19353 ) ) ;
#17185 = CARTESIAN_POINT ( 'NONE',  ( -14.00000000397460020, 22.95208919312840123, -7.999999999996929567 ) ) ;
#17186 = AXIS2_PLACEMENT_3D ( 'NONE', #16422, #21992, #1813 ) ;
#17187 = MANIFOLD_SOLID_BREP ( 'Imported1', #6098 ) ;
#17188 = AXIS2_PLACEMENT_3D ( 'NONE', #16196, #14411, #2532 ) ;
#17189 = PLANE ( 'NONE',  #18240 ) ;
#17190 = ORIENTED_EDGE ( 'NONE', *, *, #14337, .T. ) ;
#17191 = DIRECTION ( 'NONE',  ( 0.000000000000000000, -2.738683416504465444E-14, 1.000000000000000000 ) ) ;
#17192 = DIRECTION ( 'NONE',  ( -0.9999862922474492821, -0.005235963827121951387, 1.187304881134294758E-16 ) ) ;
#17193 = EDGE_CURVE ( 'NONE', #22740, #3573, #8873, .T. ) ;
#17194 = EDGE_CURVE ( 'NONE', #5941, #4383, #9325, .T. ) ;
#17195 = UNCERTAINTY_MEASURE_WITH_UNIT (LENGTH_MEASURE( 1.000000000000000082E-05 ), #14656, 'distance_accuracy_value', 'NONE');
#17196 = APPROVAL_ROLE ( '' ) ;
#17197 = DIRECTION ( 'NONE',  ( -2.982858504577314686E-17, 2.441916418604790135E-15, 1.000000000000000000 ) ) ;
#17198 = EDGE_LOOP ( 'NONE', ( #10319, #14570 ) ) ;
#17199 = VECTOR ( 'NONE', #12026, 1000.000000000000000 ) ;
#17200 = ORIENTED_EDGE ( 'NONE', *, *, #16476, .T. ) ;
#17201 = CIRCLE ( 'NONE', #5059, 2.499999999999998668 ) ;
#17202 = APPLICATION_PROTOCOL_DEFINITION ( 'international standard', 'config_control_design', 1994, #16259 ) ;
#17203 = DIRECTION ( 'NONE',  ( 0.8686315144360597928, -0.4954586684361442783, -1.318113719833499867E-16 ) ) ;
#17204 = CC_DESIGN_APPROVAL ( #11279, ( #5445 ) ) ;
#17205 = ORIENTED_EDGE ( 'NONE', *, *, #6964, .T. ) ;
#17206 = VERTEX_POINT ( 'NONE', #165 ) ;
#17207 = DIRECTION ( 'NONE',  ( 0.9730401042858024541, -0.2306359803922080898, -5.959266323858942451E-17 ) ) ;
#17208 = APPROVAL_STATUS ( 'not_yet_approved' ) ;
#17209 = AXIS2_PLACEMENT_3D ( 'NONE', #10722, #21604, #16268 ) ;
#17210 = VECTOR ( 'NONE', #9362, 999.9999999999998863 ) ;
#17211 = AXIS2_PLACEMENT_3D ( 'NONE', #8638, #12102, #19440 ) ;
#17212 = ITEM_DEFINED_TRANSFORMATION ( 'NONE', 'NONE', #3,  #12739 ) ;
#17213 = CARTESIAN_POINT ( 'NONE',  ( 41.24356139695900225, 11.92996613406540085, 18.89999999999999858 ) ) ;
#17214 = EDGE_CURVE ( 'NONE', #14326, #7448, #7719, .T. ) ;
#17215 = FACE_OUTER_BOUND ( 'NONE', #19964, .T. ) ;
#17216 = EDGE_LOOP ( 'NONE', ( #22904, #11182 ) ) ;
#17217 = CC_DESIGN_PERSON_AND_ORGANIZATION_ASSIGNMENT ( #10329, #5089, ( #14605 ) ) ;
#17218 = PERSON_AND_ORGANIZATION ( #11966, #8758 ) ;
#17219 = AXIS2_PLACEMENT_3D ( 'NONE', #17533, #8523, #19311 ) ;
#17220 = APPROVAL ( #5804, 'UNSPECIFIED' ) ;
#17221 = VERTEX_POINT ( 'NONE', #10901 ) ;
#17222 = AXIS2_PLACEMENT_3D ( 'NONE', #13187, #11066, #18300 ) ;
#17223 = DIRECTION ( 'NONE',  ( 1.466984912809909902E-16, 2.805478249466345005E-20, 1.000000000000000000 ) ) ;
#17224 = DIRECTION ( 'NONE',  ( 0.000000000000000000, -1.000000000000000000, 9.876950852243829821E-14 ) ) ;
#17225 = ORIENTED_EDGE ( 'NONE', *, *, #6545, .T. ) ;
#17226 = EDGE_CURVE ( 'NONE', #306, #19524, #7432, .T. ) ;
#17227 = EDGE_CURVE ( 'NONE', #22935, #18764, #2792, .T. ) ;
#17228 = CARTESIAN_POINT ( 'NONE',  ( -20.00000000000000000, -20.00000000000000000, 5.500000000004559020 ) ) ;
#17229 = ADVANCED_FACE ( 'NONE', ( #5636 ), #14430, .F. ) ;
#17230 = LINE ( 'NONE', #4626, #13817 ) ;
#17231 = CARTESIAN_POINT ( 'NONE',  ( -25.44839750738890061, 25.46504853262640111, -2.500000000000059952 ) ) ;
#17232 = EDGE_LOOP ( 'NONE', ( #6513, #327, #22036, #9425, #3049 ) ) ;
#17233 = ORIENTED_EDGE ( 'NONE', *, *, #7221, .T. ) ;
#17234 = EDGE_CURVE ( 'NONE', #15046, #1783, #16551, .T. ) ;
#17235 = CARTESIAN_POINT ( 'NONE',  ( -12.20588344543568837, 18.98041049132002556, -2.856163744861079589E-15 ) ) ;
#17236 = ORIENTED_EDGE ( 'NONE', *, *, #8037, .F. ) ;
#17237 = CALENDAR_DATE ( 2026, 31, 10 ) ;
#17238 = EDGE_CURVE ( 'NONE', #20661, #10873, #14780, .T. ) ;
#17239 = ORIENTED_EDGE ( 'NONE', *, *, #12665, .T. ) ;
#17240 = VERTEX_POINT ( 'NONE', #1190 ) ;
#17241 = PLANE ( 'NONE',  #10740 ) ;
#17242 = CALENDAR_DATE ( 2026, 31, 10 ) ;
#17243 = VECTOR ( 'NONE', #23326, 1000.000000000000227 ) ;
#17244 = FACE_OUTER_BOUND ( 'NONE', #17282, .T. ) ;
#17245 = CIRCLE ( 'NONE', #7009, 3.500000000000001332 ) ;
#17246 = ADVANCED_FACE ( 'NONE', ( #20477 ), #22245, .T. ) ;
#17247 = CARTESIAN_POINT ( 'NONE',  ( 0.000000000000000000, 0.000000000000000000, 0.000000000000000000 ) ) ;
#17248 = CARTESIAN_POINT ( 'NONE',  ( 59.43368109719860826, 4.124228161845699958, 3.772686752615189359E-14 ) ) ;
#17249 = COORDINATED_UNIVERSAL_TIME_OFFSET ( 0, 0, .AHEAD. ) ;
#17250 = ORIENTED_EDGE ( 'NONE', *, *, #1498, .T. ) ;
#17251 = DIRECTION ( 'NONE',  ( 3.210834492181045054E-17, -2.441916418604790135E-15, -1.000000000000000000 ) ) ;
#17252 = DIRECTION ( 'NONE',  ( 0.000000000000000000, 0.000000000000000000, 1.000000000000000000 ) ) ;
#17253 = ORIENTED_EDGE ( 'NONE', *, *, #5626, .F. ) ;
#17254 = EDGE_CURVE ( 'NONE', #18635, #20315, #11157, .T. ) ;
#17255 = EDGE_CURVE ( 'NONE', #2924, #8909, #7359, .T. ) ;
#17256 = LINE ( 'NONE', #13805, #22644 ) ;
#17257 = SPHERICAL_SURFACE ( 'NONE', #20566, 8.000000000000000000 ) ;
#17258 = VERTEX_POINT ( 'NONE', #3975 ) ;
#17259 = DIRECTION ( 'NONE',  ( 0.000000000000000000, 0.000000000000000000, -1.000000000000000000 ) ) ;
#17260 = MECHANICAL_CONTEXT ( 'NONE', #5795, 'mechanical' ) ;
#17261 = EDGE_LOOP ( 'NONE', ( #7008, #6298, #113, #22854 ) ) ;
#17262 = EDGE_LOOP ( 'NONE', ( #20660, #2020, #1103, #6631 ) ) ;
#17263 = DIRECTION ( 'NONE',  ( 0.000000000000000000, -1.000000000000000000, 2.081668171172169697E-15 ) ) ;
#17264 = DIRECTION ( 'NONE',  ( 1.159535895544890222E-14, 2.167612681253619929E-15, 1.000000000000000000 ) ) ;
#17265 = VERTEX_POINT ( 'NONE', #2982 ) ;
#17266 = APPROVAL_ROLE ( '' ) ;
#17267 = FACE_OUTER_BOUND ( 'NONE', #17702, .T. ) ;
#17268 = PERSON_AND_ORGANIZATION ( #19300, #14007 ) ;
#17269 = CARTESIAN_POINT ( 'NONE',  ( 114.8905747189829896, 12.63019305843990026, 2.920919059678259917E-14 ) ) ;
#17270 = EDGE_CURVE ( 'NONE', #11391, #4850, #16822, .T. ) ;
#17271 = AXIS2_PLACEMENT_3D ( 'NONE', #22998, #19331, #21219 ) ;
#17272 = DIRECTION ( 'NONE',  ( 0.000000000000000000, 1.668003342285391304E-16, 1.000000000000000000 ) ) ;
#17273 = CALENDAR_DATE ( 2026, 31, 10 ) ;
#17274 = LINE ( 'NONE', #8247, #10645 ) ;
#17275 = CARTESIAN_POINT ( 'NONE',  ( 39.74442752440959481, 5.605205456207779768, 19.59999999999999787 ) ) ;
#17276 = ADVANCED_FACE ( 'NONE', ( #10134 ), #5995, .F. ) ;
#17277 = CARTESIAN_POINT ( 'NONE',  ( 31.45181451370270054, 16.90945435098589655, 25.00000000000000000 ) ) ;
#17278 = DIRECTION ( 'NONE',  ( -0.9999862922474491711, -0.005235963827128305680, 1.734723475976808327E-16 ) ) ;
#17279 = ADVANCED_FACE ( 'NONE', ( #21040 ), #20364, .T. ) ;
#17280 = DIRECTION ( 'NONE',  ( 0.000000000000000000, -4.902758972191440018E-15, -1.000000000000000000 ) ) ;
#17281 = LINE ( 'NONE', #17511, #8826 ) ;
#17282 = EDGE_LOOP ( 'NONE', ( #5553, #20435, #12978, #23351 ) ) ;
#17283 = PERSON ( 'NAUO-PER17', 'UNSPECIFIED', 'UNSPECIFIED', ('UNSPECIFIED'), ('UNSPECIFIED'), ('UNSPECIFIED') ) ;
#17284 = CIRCLE ( 'NONE', #11995, 2.500000000000000444 ) ;
#17285 = ORIENTED_EDGE ( 'NONE', *, *, #18811, .F. ) ;
#17286 = CARTESIAN_POINT ( 'NONE',  ( 90.25841307858064511, 13.00434284682856045, 12.99999999999970157 ) ) ;
#17287 = CARTESIAN_POINT ( 'NONE',  ( -20.00000000000000000, -20.00000000000000000, -4.999999999995470290 ) ) ;
#17288 = ORIENTED_EDGE ( 'NONE', *, *, #19946, .F. ) ;
#17289 = CARTESIAN_POINT ( 'NONE',  ( 37.46113131852559519, -4.027891576222994985, 13.00000000000000000 ) ) ;
#17290 = ORIENTED_EDGE ( 'NONE', *, *, #6902, .T. ) ;
#17291 = DIRECTION ( 'NONE',  ( -1.000000000000000000, 0.000000000000000000, 0.000000000000000000 ) ) ;
#17292 = PERSON_AND_ORGANIZATION ( #11966, #8758 ) ;
#17293 = CARTESIAN_POINT ( 'NONE',  ( 34.07549947545469848, 22.01160333750100051, 11.50000000000000000 ) ) ;
#17294 = PRODUCT_DEFINITION_SHAPE ( 'NONE', 'NONE',  #23483 ) ;
#17295 = CONTEXT_DEPENDENT_SHAPE_REPRESENTATION ( #4124, #5894 ) ;
#17296 = DIRECTION ( 'NONE',  ( 1.000000000000000000, 0.000000000000000000, 0.000000000000000000 ) ) ;
#17297 = CARTESIAN_POINT ( 'NONE',  ( -30.79177721110609767, 6.338862259904598950, -2.999707106781169585 ) ) ;
#17298 = CC_DESIGN_PERSON_AND_ORGANIZATION_ASSIGNMENT ( #9056, #18559, ( #12933 ) ) ;
#17299 = DIRECTION ( 'NONE',  ( -0.2306359803922030105, -0.9730401042858034533, 0.000000000000000000 ) ) ;
#17300 = DIRECTION ( 'NONE',  ( 0.000000000000000000, 0.000000000000000000, 1.000000000000000000 ) ) ;
#17301 = AXIS2_PLACEMENT_3D ( 'NONE', #9053, #19512, #10503 ) ;
#17302 = DIRECTION ( 'NONE',  ( -0.2306359803922054252, -0.9730401042858028982, 0.000000000000000000 ) ) ;
#17303 = ORIENTED_EDGE ( 'NONE', *, *, #14363, .T. ) ;
#17304 = LINE ( 'NONE', #10307, #12078 ) ;
#17305 = AXIS2_PLACEMENT_3D ( 'NONE', #11361, #3974, #7655 ) ;
#17306 = MANIFOLD_SOLID_BREP ( 'Imported1', #6403 ) ;
#17307 = DIRECTION ( 'NONE',  ( -0.9730401042858024541, 0.2306359803922080898, 5.959266323858942451E-17 ) ) ;
#17308 = ORIENTED_EDGE ( 'NONE', *, *, #2678, .T. ) ;
#17309 = CARTESIAN_POINT ( 'NONE',  ( 35.93754633002667731, 11.81769736674259086, -8.759424124907059905 ) ) ;
#17310 = CARTESIAN_POINT ( 'NONE',  ( -24.50000000000000000, -31.09999999999999787, 19.00000000000000000 ) ) ;
#17311 = PERSON_AND_ORGANIZATION_ROLE ( 'classification_officer' ) ;
#17312 = DIRECTION ( 'NONE',  ( 9.248937406224699144E-11, -1.000000000000000000, 2.220446028257580150E-15 ) ) ;
#17313 = ORIENTED_EDGE ( 'NONE', *, *, #7026, .T. ) ;
#17314 = ORIENTED_EDGE ( 'NONE', *, *, #16245, .F. ) ;
#17315 = APPROVAL_ROLE ( '' ) ;
#17316 = DIRECTION ( 'NONE',  ( 0.9999862922474493931, 0.005235963827108502076, 0.000000000000000000 ) ) ;
#17317 = EDGE_CURVE ( 'NONE', #20134, #4119, #13128, .T. ) ;
#17318 = ORIENTED_EDGE ( 'NONE', *, *, #7412, .T. ) ;
#17319 = VECTOR ( 'NONE', #16577, 1000.000000000000114 ) ;
#17320 = AXIS2_PLACEMENT_3D ( 'NONE', #1219, #8492, #3819 ) ;
#17321 = DIRECTION ( 'NONE',  ( -0.9730401042858022320, 0.2306359803922080343, 5.959266323858941219E-17 ) ) ;
#17322 = DATE_AND_TIME ( #6639, #10365 ) ;
#17323 = PERSON_AND_ORGANIZATION ( #287, #13707 ) ;
#17324 = DIRECTION ( 'NONE',  ( 0.9999862922474492821, 0.005235963827121822151, -1.187304881134280213E-16 ) ) ;
#17325 = DIRECTION ( 'NONE',  ( -0.9730401042858024541, 0.2306359803922080898, 5.959266323858942451E-17 ) ) ;
#17326 = ORIENTED_EDGE ( 'NONE', *, *, #5199, .F. ) ;
#17327 = COORDINATED_UNIVERSAL_TIME_OFFSET ( 0, 0, .AHEAD. ) ;
#17328 = AXIS2_PLACEMENT_3D ( 'NONE', #6364, #13846, #13604 ) ;
#17329 = AXIS2_PLACEMENT_3D ( 'NONE', #3070, #1157, #23249 ) ;
#17330 = CIRCLE ( 'NONE', #10533, 2.500000000000000444 ) ;
#17331 = ORIENTED_EDGE ( 'NONE', *, *, #10962, .T. ) ;
#17332 = CARTESIAN_POINT ( 'NONE',  ( -3.499952022866071655, -0.01832587339492760051, -2.500000000000089706 ) ) ;
#17333 = CARTESIAN_POINT ( 'NONE',  ( 2.671834669462810119, 17.57827187707419725, -6.695602606842560264E-15 ) ) ;
#17334 = ORIENTED_EDGE ( 'NONE', *, *, #11551, .T. ) ;
#17335 = CARTESIAN_POINT ( 'NONE',  ( -17.50000000000000000, -19.99999998334472195, 6.750000000004530598 ) ) ;
#17336 = FACE_OUTER_BOUND ( 'NONE', #10965, .T. ) ;
#17337 = DIRECTION ( 'NONE',  ( -1.000000000000000000, 2.270069654138870255E-15, -3.099353312215988811E-62 ) ) ;
#17338 = ORIENTED_EDGE ( 'NONE', *, *, #3026, .T. ) ;
#17339 = VERTEX_POINT ( 'NONE', #18724 ) ;
#17340 = FACE_OUTER_BOUND ( 'NONE', #14870, .T. ) ;
#17341 = ORIENTED_EDGE ( 'NONE', *, *, #13204, .F. ) ;
#17342 = APPLICATION_PROTOCOL_DEFINITION ( 'international standard', 'config_control_design', 1994, #19912 ) ;
#17343 = ADVANCED_FACE ( 'NONE', ( #5879, #15701 ), #17472, .T. ) ;
#17344 = MANIFOLD_SOLID_BREP ( 'Imported1', #9444 ) ;
#17345 = VERTEX_POINT ( 'NONE', #396 ) ;
#17346 = ORIENTED_EDGE ( 'NONE', *, *, #17179, .T. ) ;
#17347 = DIRECTION ( 'NONE',  ( -3.210834492181045054E-17, 2.441916418604790135E-15, 1.000000000000000000 ) ) ;
#17348 = VECTOR ( 'NONE', #1692, 1000.000000000000000 ) ;
#17349 = APPROVAL_ROLE ( '' ) ;
#17350 = APPROVAL ( #8130, 'UNKNOWN' ) ;
#17351 = AXIS2_PLACEMENT_3D ( 'NONE', #12195, #3154, #6838 ) ;
#17352 = PLANE ( 'NONE',  #3645 ) ;
#17353 = CIRCLE ( 'NONE', #7114, 4.349999999999996980 ) ;
#17354 = EDGE_CURVE ( 'NONE', #22503, #21418, #105, .T. ) ;
#17355 = EDGE_CURVE ( 'NONE', #18172, #10377, #23256, .T. ) ;
#17356 = AXIS2_PLACEMENT_3D ( 'NONE', #1584, #7184, #10771 ) ;
#17357 =( REPRESENTATION_RELATIONSHIP ('NONE','NONE', #19303, #5493 ) REPRESENTATION_RELATIONSHIP_WITH_TRANSFORMATION ( #669 )SHAPE_REPRESENTATION_RELATIONSHIP( ) );
#17358 = CARTESIAN_POINT ( 'NONE',  ( -30.79248430819469817, 6.338858557518999959, -3.000000000000079936 ) ) ;
#17359 = CALENDAR_DATE ( 2026, 31, 10 ) ;
#17360 = ORIENTED_EDGE ( 'NONE', *, *, #8984, .F. ) ;
#17361 = AXIS2_PLACEMENT_3D ( 'NONE', #7722, #22307, #15189 ) ;
#17362 = CARTESIAN_POINT ( 'NONE',  ( 36.57467860885130051, 21.71590586959130320, -15.00000000000049916 ) ) ;
#17363 = FACE_OUTER_BOUND ( 'NONE', #2669, .T. ) ;
#17364 = ORIENTED_EDGE ( 'NONE', *, *, #7830, .F. ) ;
#17365 = LINE ( 'NONE', #22928, #8259 ) ;
#17367 = AXIS2_PLACEMENT_3D ( 'NONE', #5061, #21083, #13962 ) ;
#17366 = CARTESIAN_POINT ( 'NONE',  ( 35.59419854219520118, 9.774809681453469068, 10.99076000000020059 ) ) ;
#17368 = DIRECTION ( 'NONE',  ( 0.000000000000000000, 1.000000000000000000, 0.000000000000000000 ) ) ;
#17369 = ORIENTED_EDGE ( 'NONE', *, *, #18380, .F. ) ;
#17370 = CYLINDRICAL_SURFACE ( 'NONE', #10361, 3.500000000000000444 ) ;
#17371 = DATE_AND_TIME ( #15814, #4203 ) ;
#17372 = EDGE_CURVE ( 'NONE', #6910, #10876, #6682, .T. ) ;
#17373 = ORIENTED_EDGE ( 'NONE', *, *, #19989, .F. ) ;
#17374 = ORIENTED_EDGE ( 'NONE', *, *, #2518, .T. ) ;
#17375 = CARTESIAN_POINT ( 'NONE',  ( -20.00000000000149925, -20.00000000000000000, -6.499999999995289990 ) ) ;
#17376 = DIRECTION ( 'NONE',  ( 8.911056267098788616E-18, 1.998401444326210262E-15, 1.000000000000000000 ) ) ;
#17377 = ORIENTED_EDGE ( 'NONE', *, *, #7066, .F. ) ;
#17378 = AXIS2_PLACEMENT_3D ( 'NONE', #22376, #9336, #5770 ) ;
#17379 = PERSON_AND_ORGANIZATION_ROLE ( 'design_supplier' ) ;
#17380 = PLANE ( 'NONE',  #10009 ) ;
#17381 = APPROVAL ( #22996, 'UNSPECIFIED' ) ;
#17382 = APPROVAL ( #19610, 'UNSPECIFIED' ) ;
#17383 = CARTESIAN_POINT ( 'NONE',  ( -26.00000000397409750, 22.95208919201850151, -5.499999999994199307 ) ) ;
#17384 = VECTOR ( 'NONE', #11900, 1000.000000000000000 ) ;
#17385 = APPROVAL_STATUS ( 'not_yet_approved' ) ;
#17386 = DIRECTION ( 'NONE',  ( 0.000000000000000000, 0.000000000000000000, -1.000000000000000000 ) ) ;
#17387 = EDGE_CURVE ( 'NONE', #15347, #15675, #1638, .T. ) ;
#17388 = ADVANCED_FACE ( 'NONE', ( #20606 ), #2190, .T. ) ;
#17389 = MANIFOLD_SOLID_BREP ( 'Imported1', #1457 ) ;
#17390 = VECTOR ( 'NONE', #7280, 999.9999999999998863 ) ;
#17391 = CARTESIAN_POINT ( 'NONE',  ( -20.00000000000000000, -17.50000000000000000, 5.500000000004554579 ) ) ;
#17392 = APPROVAL_DATE_TIME ( #19174, #1159 ) ;
#17393 = CARTESIAN_POINT ( 'NONE',  ( 37.28322146592795150, 10.97386708096955665, 8.864945788362589951 ) ) ;
#17394 = CARTESIAN_POINT ( 'NONE',  ( 52.73786095581300515, -7.648876468381259564, -13.00000000000039968 ) ) ;
#17395 = DIRECTION ( 'NONE',  ( -0.2306359803922028162, -0.9730401042858034533, 1.407521210652564497E-17 ) ) ;
#17396 = DIRECTION ( 'NONE',  ( -1.000000000000000000, 0.000000000000000000, 0.000000000000000000 ) ) ;
#17397 = FACE_OUTER_BOUND ( 'NONE', #4971, .T. ) ;
#17398 = FACE_OUTER_BOUND ( 'NONE', #18630, .T. ) ;
#17399 = VERTEX_POINT ( 'NONE', #9570 ) ;
#17400 = EDGE_CURVE ( 'NONE', #18339, #4805, #1274, .T. ) ;
#17401 = EDGE_LOOP ( 'NONE', ( #13433, #16188, #13199, #15898 ) ) ;
#17402 = CARTESIAN_POINT ( 'NONE',  ( 35.59419854219520118, 9.774809681453550780, 27.87500000000000000 ) ) ;
#17403 = DIRECTION ( 'NONE',  ( -0.2306359803922025109, -0.9730401042858035643, 5.112869192352692394E-15 ) ) ;
#17404 = ORIENTED_EDGE ( 'NONE', *, *, #8399, .F. ) ;
#17405 = CARTESIAN_POINT ( 'NONE',  ( 35.59419854219520118, 9.774809681453278998, -23.00000000000000000 ) ) ;
#17406 = ORIENTED_EDGE ( 'NONE', *, *, #19277, .T. ) ;
#17407 = DIRECTION ( 'NONE',  ( 0.9730401042858035643, -0.2306359803922028717, -5.959266323858674978E-17 ) ) ;
#17408 = PERSON_AND_ORGANIZATION ( #11966, #8758 ) ;
#17409 = CARTESIAN_POINT ( 'NONE',  ( 28.89837840081079889, -1.998294948772169954, 13.00000000000019895 ) ) ;
#17410 = EDGE_CURVE ( 'NONE', #22086, #23172, #4771, .T. ) ;
#17411 = EDGE_CURVE ( 'NONE', #20776, #16195, #22138, .T. ) ;
#17412 = CALENDAR_DATE ( 2026, 31, 10 ) ;
#17413 = DIRECTION ( 'NONE',  ( 0.000000000000000000, 0.000000000000000000, 1.000000000000000000 ) ) ;
#17414 = DIRECTION ( 'NONE',  ( -0.9730401042858024541, 0.2306359803922080898, 5.959266323858942451E-17 ) ) ;
#17415 = DIRECTION ( 'NONE',  ( 1.138590270679730064E-14, 2.220446049251240387E-15, 1.000000000000000000 ) ) ;
#17416 = CARTESIAN_POINT ( 'NONE',  ( 36.30836311812279860, 20.59233593730780143, -13.00000000000049916 ) ) ;
#17417 = ORIENTED_EDGE ( 'NONE', *, *, #8671, .F. ) ;
#17418 = FACE_OUTER_BOUND ( 'NONE', #18657, .T. ) ;
#17419 = LINE ( 'NONE', #22874, #21283 ) ;
#17420 = EDGE_LOOP ( 'NONE', ( #22167, #212, #4891, #6920, #6986, #19044, #14368, #22173 ) ) ;
#17421 = CARTESIAN_POINT ( 'NONE',  ( 33.90636897763663882, 8.573931448519822140, -8.864692334380263716 ) ) ;
#17422 = AXIS2_PLACEMENT_3D ( 'NONE', #21304, #1461, #10415 ) ;
#17423 = FACE_OUTER_BOUND ( 'NONE', #7844, .T. ) ;
#17424 = DIRECTION ( 'NONE',  ( 1.000000000000000000, -2.270069654138870255E-15, 3.099353312215988811E-62 ) ) ;
#17425 = EDGE_LOOP ( 'NONE', ( #16810, #17360, #6679, #23318 ) ) ;
#17426 = ORIENTED_EDGE ( 'NONE', *, *, #6267, .F. ) ;
#17427 = APPROVAL ( #13904, 'UNSPECIFIED' ) ;
#17428 = APPROVAL_ROLE ( '' ) ;
#17429 = CARTESIAN_POINT ( 'NONE',  ( 66.60056952104010008, 2.425487965306460048, 1.173314102775059961E-14 ) ) ;
#17430 = ORIENTED_EDGE ( 'NONE', *, *, #4613, .F. ) ;
#17431 = CARTESIAN_POINT ( 'NONE',  ( -20.00000000000000000, -20.00000000000000000, -5.499999999995469402 ) ) ;
#17432 = CALENDAR_DATE ( 2026, 31, 10 ) ;
#17433 = PRODUCT_DEFINITION_SHAPE ( 'NONE', 'NONE',  #16771 ) ;
#17434 = CALENDAR_DATE ( 2026, 31, 10 ) ;
#17435 = CARTESIAN_POINT ( 'NONE',  ( -26.00000000397269773, 22.95208919201850151, 8.000000000004529710 ) ) ;
#17436 = CC_DESIGN_APPROVAL ( #9960, ( #11759 ) ) ;
#17437 = DIRECTION ( 'NONE',  ( -7.440628469791170033E-16, -2.880774829024070580E-15, -1.000000000000000000 ) ) ;
#17438 = VERTEX_POINT ( 'NONE', #7147 ) ;
#17439 = ADVANCED_FACE ( 'NONE', ( #14373 ), #14027, .T. ) ;
#17440 = VERTEX_POINT ( 'NONE', #3221 ) ;
#17441 = CARTESIAN_POINT ( 'NONE',  ( -12.50000000434259917, 26.95208919326709918, 8.000000000004369838 ) ) ;
#17442 = CARTESIAN_POINT ( 'NONE',  ( 63.86158900585790832, 8.213232408304289578, 1.054077144304177353E-14 ) ) ;
#17443 = ORIENTED_EDGE ( 'NONE', *, *, #3312, .T. ) ;
#17444 = CYLINDRICAL_SURFACE ( 'NONE', #21527, 2.499999999999998668 ) ;
#17445 = DIRECTION ( 'NONE',  ( 2.269747459788999852E-13, 2.220446049250470459E-15, 1.000000000000000000 ) ) ;
#17446 = CARTESIAN_POINT ( 'NONE',  ( 28.89837840081079889, -1.998294948772289858, -13.00000000000039968 ) ) ;
#17447 = CIRCLE ( 'NONE', #1495, 2.500000000000000000 ) ;
#17448 = EDGE_LOOP ( 'NONE', ( #2101, #7090, #22695, #10541 ) ) ;
#17449 = ORIENTED_EDGE ( 'NONE', *, *, #21947, .T. ) ;
#17451 = VECTOR ( 'NONE', #8433, 1000.000000000000000 ) ;
#17450 = CARTESIAN_POINT ( 'NONE',  ( 114.3964932440919995, -22.26358663789240211, 13.00000000000000000 ) ) ;
#17452 = ORIENTED_EDGE ( 'NONE', *, *, #7067, .F. ) ;
#17453 = PERSON_AND_ORGANIZATION_ROLE ( 'design_supplier' ) ;
#17454 = ORIENTED_EDGE ( 'NONE', *, *, #3854, .T. ) ;
#17455 = ORIENTED_EDGE ( 'NONE', *, *, #2300, .F. ) ;
#17456 = DIRECTION ( 'NONE',  ( -0.2867834340965179085, 0.9579954394086686031, 0.000000000000000000 ) ) ;
#17457 = DATE_TIME_ROLE ( 'creation_date' ) ;
#17458 = AXIS2_PLACEMENT_3D ( 'NONE', #10624, #19875, #9057 ) ;
#17459 = DIRECTION ( 'NONE',  ( -0.9730401042858036753, 0.2306359803922031493, -2.740969466505752002E-16 ) ) ;
#17460 = LOCAL_TIME ( 14, 11, 27.00000000000000000, #17115 ) ;
#17461 = AXIS2_PLACEMENT_3D ( 'NONE', #16849, #21320, #12328 ) ;
#17462 = PLANE ( 'NONE',  #23236 ) ;
#17463 = DIRECTION ( 'NONE',  ( -0.005235963827101452160, 0.9999862922474493931, 5.492442074325202057E-16 ) ) ;
#17464 = ADVANCED_FACE ( 'NONE', ( #23278 ), #3449, .T. ) ;
#17465 = DATE_TIME_ROLE ( 'creation_date' ) ;
#17466 = ORIENTED_EDGE ( 'NONE', *, *, #13270, .T. ) ;
#17467 = DIRECTION ( 'NONE',  ( -1.248400535696349791E-16, 3.446306084657139973E-17, 1.000000000000000000 ) ) ;
#17468 = CARTESIAN_POINT ( 'NONE',  ( 31.11077410011089839, -1.335996977273150144, 15.00000000000000000 ) ) ;
#17469 = AXIS2_PLACEMENT_3D ( 'NONE', #21385, #1767, #14141 ) ;
#17470 = ORIENTED_EDGE ( 'NONE', *, *, #6303, .F. ) ;
#17471 = DIRECTION ( 'NONE',  ( -1.000000000000000000, -6.662111140531837817E-09, 1.110223024625157172E-14 ) ) ;
#17472 = PLANE ( 'NONE',  #2423 ) ;
#17473 = DIRECTION ( 'NONE',  ( 0.9999862922474493931, 0.005235963827110170880, 0.000000000000000000 ) ) ;
#17474 = VERTEX_POINT ( 'NONE', #12380 ) ;
#17475 = LINE ( 'NONE', #10137, #828 ) ;
#17476 = APPLICATION_CONTEXT ( 'configuration controlled 3d designs of mechanical parts and assemblies' ) ;
#17477 = ADVANCED_FACE ( 'NONE', ( #17957 ), #9037, .T. ) ;
#17478 = ADVANCED_FACE ( 'NONE', ( #18061 ), #20640, .F. ) ;
#17479 = CALENDAR_DATE ( 2026, 31, 10 ) ;
#17480 = LOCAL_TIME ( 14, 11, 27.00000000000000000, #23284 ) ;
#17481 = ORIENTED_EDGE ( 'NONE', *, *, #13991, .T. ) ;
#17482 = ORIENTED_EDGE ( 'NONE', *, *, #22013, .T. ) ;
#17483 = CARTESIAN_POINT ( 'NONE',  ( -20.00000000000180123, -20.00000000000000000, -7.999999999995469402 ) ) ;
#17484 = CARTESIAN_POINT ( 'NONE',  ( 118.5310588935630136, -6.697506338400819992, 20.00000000000000000 ) ) ;
#17485 = LOCAL_TIME ( 14, 11, 27.00000000000000000, #21783 ) ;
#17486 = CARTESIAN_POINT ( 'NONE',  ( -8.080225385240000335, -15.72171916155420313, -2.500000000000000000 ) ) ;
#17487 = DATE_AND_TIME ( #3231, #4255 ) ;
#17488 = DIRECTION ( 'NONE',  ( 0.9730401042858035643, -0.2306359803922031215, 1.084982917713590597E-15 ) ) ;
#17489 = VECTOR ( 'NONE', #8165, 999.9999999999998863 ) ;
#17490 = LOCAL_TIME ( 14, 11, 27.00000000000000000, #23223 ) ;
#17491 = LINE ( 'NONE', #2776, #23402 ) ;
#17492 = CARTESIAN_POINT ( 'NONE',  ( 34.14207834813680620, 22.29249582057189727, 11.00000000000000000 ) ) ;
#17493 = CIRCLE ( 'NONE', #14030, 2.499999999999998224 ) ;
#17494 =( BOUNDED_CURVE ( )  B_SPLINE_CURVE ( 2, ( #10388, #12287, #22697 ),
 .UNSPECIFIED., .F., .F. ) 
 B_SPLINE_CURVE_WITH_KNOTS ( ( 3, 3 ),
 ( 0.000000000000000000, 0.2336872276155859962 ),
 .UNSPECIFIED. ) 
 CURVE ( )  GEOMETRIC_REPRESENTATION_ITEM ( )  RATIONAL_B_SPLINE_CURVE ( ( 1.000000000000000000, 1.154700538379249908, 1.000000000000000000 ) ) 
 REPRESENTATION_ITEM ( '' )  );
#17495 = DIRECTION ( 'NONE',  ( -0.005235963827117002221, 0.9999862922474493931, 2.636227439667000721E-16 ) ) ;
#17496 = EDGE_CURVE ( 'NONE', #10370, #2347, #21261, .T. ) ;
#17497 = COORDINATED_UNIVERSAL_TIME_OFFSET ( 0, 0, .AHEAD. ) ;
#17498 = LOCAL_TIME ( 14, 11, 27.00000000000000000, #20779 ) ;
#17499 = LOCAL_TIME ( 14, 11, 27.00000000000000000, #8106 ) ;
#17500 = DIRECTION ( 'NONE',  ( -0.2306359803922066187, -0.9730401042858026761, 0.000000000000000000 ) ) ;
#17501 = CIRCLE ( 'NONE', #9943, 5.999999999999999112 ) ;
#17502 = CARTESIAN_POINT ( 'NONE',  ( -27.00000000000000000, -30.47499999999999787, -19.00000000000000000 ) ) ;
#17503 = CC_DESIGN_PERSON_AND_ORGANIZATION_ASSIGNMENT ( #20490, #11502, ( #4576 ) ) ;
#17504 = EDGE_CURVE ( 'NONE', #21288, #4764, #15921, .T. ) ;
#17505 = PLANE ( 'NONE',  #17320 ) ;
#17506 = DIRECTION ( 'NONE',  ( -0.9730401042858035643, 0.2306359803922028717, 5.958148513035547083E-17 ) ) ;
#17507 = CC_DESIGN_PERSON_AND_ORGANIZATION_ASSIGNMENT ( #23365, #5554, ( #10683 ) ) ;
#17508 = LINE ( 'NONE', #23067, #3863 ) ;
#17509 = ORIENTED_EDGE ( 'NONE', *, *, #22295, .F. ) ;
#17510 = LOCAL_TIME ( 14, 11, 27.00000000000000000, #22762 ) ;
#17511 = CARTESIAN_POINT ( 'NONE',  ( 2.500000000000026645, -7.535786464196452844E-15, 2.500000000000000000 ) ) ;
#17512 = ADVANCED_FACE ( 'NONE', ( #6796 ), #16457, .F. ) ;
#17514 = VERTEX_POINT ( 'NONE', #8925 ) ;
#17513 = EDGE_CURVE ( 'NONE', #20176, #19233, #13445, .T. ) ;
#17515 = APPROVAL ( #20417, 'UNSPECIFIED' ) ;
#17516 = ORIENTED_EDGE ( 'NONE', *, *, #23001, .T. ) ;
#17517 = CARTESIAN_POINT ( 'NONE',  ( -20.00000000000000000, -20.00000000000000000, 2.500000000000000000 ) ) ;
#17518 = FACE_OUTER_BOUND ( 'NONE', #13400, .T. ) ;
#17519 = ADVANCED_FACE ( 'NONE', ( #3102 ), #16153, .F. ) ;
#17520 = ORIENTED_EDGE ( 'NONE', *, *, #10235, .F. ) ;
#17521 = LINE ( 'NONE', #14293, #16025 ) ;
#17522 = ORIENTED_EDGE ( 'NONE', *, *, #23317, .T. ) ;
#17523 = LOCAL_TIME ( 14, 11, 27.00000000000000000, #17672 ) ;
#17524 = CARTESIAN_POINT ( 'NONE',  ( 32.96699026062352544, 10.39752682851222865, -26.50000000000050093 ) ) ;
#17525 = APPROVAL_ROLE ( '' ) ;
#17526 = AXIS2_PLACEMENT_3D ( 'NONE', #18092, #7174, #9063 ) ;
#17527 = CARTESIAN_POINT ( 'NONE',  ( 114.6071564266699880, -22.31351932764730250, -13.00000000000000000 ) ) ;
#17528 = CC_DESIGN_SECURITY_CLASSIFICATION ( #62, ( #23496 ) ) ;
#17529 = FACE_OUTER_BOUND ( 'NONE', #21823, .T. ) ;
#17530 = DIRECTION ( 'NONE',  ( 0.000000000000000000, 0.000000000000000000, -1.000000000000000000 ) ) ;
#17531 = ADVANCED_FACE ( 'NONE', ( #8580 ), #19496, .F. ) ;
#17532 = DIRECTION ( 'NONE',  ( 1.000000000000000000, 0.000000000000000000, 0.000000000000000000 ) ) ;
#17533 = CARTESIAN_POINT ( 'NONE',  ( -22.52506282043049879, 26.45208917575140006, 5.500000000004489742 ) ) ;
#17534 = ORIENTED_EDGE ( 'NONE', *, *, #12127, .F. ) ;
#17535 = FACE_OUTER_BOUND ( 'NONE', #14990, .T. ) ;
#17536 = DESIGN_CONTEXT ( 'detailed design', #8989, 'design' ) ;
#17537 = CC_DESIGN_APPROVAL ( #15886, ( #19382 ) ) ;
#17538 = CARTESIAN_POINT ( 'NONE',  ( 33.16159828148068556, 10.35139963243378602, -26.30000000000050520 ) ) ;
#17539 = ORIENTED_EDGE ( 'NONE', *, *, #21686, .F. ) ;
#17540 = FACE_OUTER_BOUND ( 'NONE', #23000, .T. ) ;
#17541 = AXIS2_PLACEMENT_3D ( 'NONE', #9670, #718, #16884 ) ;
#17542 = LINE ( 'NONE', #12100, #9527 ) ;
#17543 = ADVANCED_FACE ( 'NONE', ( #1313, #8691, #10374 ), #3578, .F. ) ;
#17544 = AXIS2_PLACEMENT_3D ( 'NONE', #16247, #2105, #308 ) ;
#17545 = ORIENTED_EDGE ( 'NONE', *, *, #18854, .F. ) ;
#17546 = ITEM_DEFINED_TRANSFORMATION ( 'NONE', 'NONE', #2866,  #12739 ) ;
#17547 = EDGE_CURVE ( 'NONE', #15073, #2908, #1771, .T. ) ;
#17548 = CONICAL_SURFACE ( 'NONE', #1212, 5.386751345948120218, 1.047197551196598297 ) ;
#17549 = AXIS2_PLACEMENT_3D ( 'NONE', #9212, #20258, #20015 ) ;
#17550 = DIRECTION ( 'NONE',  ( -0.1153179901961009640, -0.4865200521429018377, 0.8660254037844385966 ) ) ;
#17551 = ORIENTED_EDGE ( 'NONE', *, *, #892, .F. ) ;
#17552 = SECURITY_CLASSIFICATION ( '', '', #8271 ) ;
#17553 = EDGE_LOOP ( 'NONE', ( #2525, #15035, #13656, #13714, #13103, #19690 ) ) ;
#17554 = DATE_TIME_ROLE ( 'creation_date' ) ;
#17555 = AXIS2_PLACEMENT_3D ( 'NONE', #4892, #13916, #17259 ) ;
#17556 = FACE_OUTER_BOUND ( 'NONE', #12946, .T. ) ;
#17557 = ORIENTED_EDGE ( 'NONE', *, *, #9871, .F. ) ;
#17558 = DIRECTION ( 'NONE',  ( -1.187319687680494078E-16, -2.805478249478340539E-20, -1.000000000000000000 ) ) ;
#17559 = AXIS2_PLACEMENT_3D ( 'NONE', #12474, #9258, #23368 ) ;
#17560 = DATE_TIME_ROLE ( 'creation_date' ) ;
#17561 = LOCAL_TIME ( 14, 11, 27.00000000000000000, #17677 ) ;
#17562 = DATE_TIME_ROLE ( 'classification_date' ) ;
#17563 = DIRECTION ( 'NONE',  ( 0.9730401042858024541, -0.2306359803922080898, -5.959266323858942451E-17 ) ) ;
#17564 = VECTOR ( 'NONE', #17720, 1000.000000000000114 ) ;
#17565 = AXIS2_PLACEMENT_3D ( 'NONE', #14786, #3860, #169 ) ;
#17566 = CIRCLE ( 'NONE', #22855, 6.500000000000000888 ) ;
#17567 = CARTESIAN_POINT ( 'NONE',  ( 56.55073134229600385, -8.038773141726823113, 3.790339717502946186E-14 ) ) ;
#17568 = VERTEX_POINT ( 'NONE', #5125 ) ;
#17569 = ORIENTED_EDGE ( 'NONE', *, *, #17410, .T. ) ;
#17570 = AXIS2_PLACEMENT_3D ( 'NONE', #23205, #14419, #16433 ) ;
#17571 = CARTESIAN_POINT ( 'NONE',  ( -61.39998491075130005, -25.32193520680032250, -5.000000000000000888 ) ) ;
#17572 = CYLINDRICAL_SURFACE ( 'NONE', #5567, 2.499999999999998668 ) ;
#17573 = ORIENTED_EDGE ( 'NONE', *, *, #8079, .F. ) ;
#17574 = VECTOR ( 'NONE', #21253, 1000.000000000000000 ) ;
#17575 = EDGE_CURVE ( 'NONE', #21866, #20385, #18763, .T. ) ;
#17576 = CC_DESIGN_APPROVAL ( #23135, ( #10554 ) ) ;
#17577 = DIRECTION ( 'NONE',  ( -8.911056267098788616E-18, -1.998401444326210262E-15, -1.000000000000000000 ) ) ;
#17578 = CARTESIAN_POINT ( 'NONE',  ( -3.458317987535629801, 19.03127855354509990, -7.892745253163399067E-16 ) ) ;
#17579 = DIRECTION ( 'NONE',  ( -0.2306359803922025109, -0.9730401042858035643, 5.112869192352692394E-15 ) ) ;
#17580 = ORIENTED_EDGE ( 'NONE', *, *, #15661, .T. ) ;
#17581 = EDGE_LOOP ( 'NONE', ( #23288, #22044, #4944, #7662, #19269 ) ) ;
#17582 = CARTESIAN_POINT ( 'NONE',  ( -24.50000000000000000, -31.09999999999999787, -19.00000000000000000 ) ) ;
#17583 = CIRCLE ( 'NONE', #5049, 2.370000000000002771 ) ;
#17584 = ORIENTED_EDGE ( 'NONE', *, *, #15771, .T. ) ;
#17585 = VECTOR ( 'NONE', #21158, 1000.000000000000227 ) ;
#17586 = MECHANICAL_CONTEXT ( 'NONE', #6251, 'mechanical' ) ;
#17587 = ADVANCED_BREP_SHAPE_REPRESENTATION ( '', ( #16982, #12739 ), #14249 ) ;
#17588 = MANIFOLD_SOLID_BREP ( 'Imported1', #3363 ) ;
#17589 = VERTEX_POINT ( 'NONE', #8810 ) ;
#17590 = CIRCLE ( 'NONE', #6584, 4.999999999999995559 ) ;
#17591 = ORIENTED_EDGE ( 'NONE', *, *, #5759, .F. ) ;
#17592 = FACE_OUTER_BOUND ( 'NONE', #4234, .T. ) ;
#17593 = PERSON_AND_ORGANIZATION_ROLE ( 'design_owner' ) ;
#17594 = CARTESIAN_POINT ( 'NONE',  ( 5.000000000000000000, -31.09999999999999787, 6.250000000000000000 ) ) ;
#17595 = CIRCLE ( 'NONE', #5777, 2.500000000000000444 ) ;
#17596 = SECURITY_CLASSIFICATION ( '', '', #20112 ) ;
#17597 = CIRCLE ( 'NONE', #2416, 2.500000000000000000 ) ;
#17598 =( LENGTH_UNIT ( ) NAMED_UNIT ( * ) SI_UNIT ( .MILLI., .METRE. ) );
#17599 = CARTESIAN_POINT ( 'NONE',  ( 36.10037903421270755, -9.768828191507939351, 3.399999999999999911 ) ) ;
#17600 = PERSON_AND_ORGANIZATION_ROLE ( 'creator' ) ;
#17601 = CIRCLE ( 'NONE', #10412, 12.50000000000000000 ) ;
#17602 = ORIENTED_EDGE ( 'NONE', *, *, #782, .F. ) ;
#17603 = LINE ( 'NONE', #4651, #20114 ) ;
#17604 = LINE ( 'NONE', #12031, #23397 ) ;
#17605 = ORIENTED_EDGE ( 'NONE', *, *, #8323, .T. ) ;
#17606 = DIRECTION ( 'NONE',  ( 6.123230174520409620E-17, 4.962644601432260272E-15, 1.000000000000000000 ) ) ;
#17607 = DIRECTION ( 'NONE',  ( 4.115594265186587621E-36, 2.805478249468460519E-20, 1.000000000000000000 ) ) ;
#17608 = DIRECTION ( 'NONE',  ( 0.9730401042858024541, -0.2306359803922080898, -5.959266323858942451E-17 ) ) ;
#17609 = ORIENTED_EDGE ( 'NONE', *, *, #449, .F. ) ;
#17610 = DIRECTION ( 'NONE',  ( -0.2306359803922077290, -0.9730401042858024541, 0.000000000000000000 ) ) ;
#17611 = APPROVAL_DATE_TIME ( #17371, #11882 ) ;
#17612 = AXIS2_PLACEMENT_3D ( 'NONE', #160, #273, #13005 ) ;
#17613 = ORIENTED_EDGE ( 'NONE', *, *, #10986, .T. ) ;
#17614 = ORIENTED_EDGE ( 'NONE', *, *, #20920, .F. ) ;
#17615 = DIRECTION ( 'NONE',  ( -1.000000000000000000, 0.000000000000000000, 1.187319687680499994E-16 ) ) ;
#17616 = CARTESIAN_POINT ( 'NONE',  ( -57.82789425897600211, 8.093822260023562976, 2.213507334852099266E-15 ) ) ;
#17617 = AXIS2_PLACEMENT_3D ( 'NONE', #3335, #10602, #1541 ) ;
#17618 = PERSON_AND_ORGANIZATION ( #11966, #8758 ) ;
#17619 = ADVANCED_FACE ( 'NONE', ( #1891 ), #11310, .F. ) ;
#17620 = CARTESIAN_POINT ( 'NONE',  ( 114.3964932440919995, -22.26358663789240211, -13.00000000000000000 ) ) ;
#17621 = EDGE_CURVE ( 'NONE', #10873, #11427, #9387, .T. ) ;
#17622 = PLANE ( 'NONE',  #12553 ) ;
#17623 = DIRECTION ( 'NONE',  ( 1.460648829817079213E-31, -3.848888668432490244E-16, 1.000000000000000000 ) ) ;
#17624 = CARTESIAN_POINT ( 'NONE',  ( 0.000000000000000000, 0.000000000000000000, 0.000000000000000000 ) ) ;
#17625 = EDGE_CURVE ( 'NONE', #18146, #11749, #3185, .T. ) ;
#17626 = ADVANCED_FACE ( 'NONE', ( #16608 ), #332, .T. ) ;
#17627 = CARTESIAN_POINT ( 'NONE',  ( 120.6036919168680015, 2.985523383783569962, 13.00000000000000000 ) ) ;
#17628 = PERSON_AND_ORGANIZATION ( #11966, #8758 ) ;
#17629 = CARTESIAN_POINT ( 'NONE',  ( 55.46237324781409939, -8.294657213477510282, 13.00000000000000000 ) ) ;
#17630 = CARTESIAN_POINT ( 'NONE',  ( -30.15694676875160241, 9.287188980624559775, 2.500000000000000000 ) ) ;
#17631 = APPLICATION_CONTEXT ( 'configuration controlled 3d designs of mechanical parts and assemblies' ) ;
#17632 = DIRECTION ( 'NONE',  ( 1.000000000000000000, -1.380319151415139905E-18, 0.000000000000000000 ) ) ;
#17633 = DIRECTION ( 'NONE',  ( -2.269747459788994803E-13, -2.220446049250320181E-15, -1.000000000000000000 ) ) ;
#17634 = CARTESIAN_POINT ( 'NONE',  ( -20.00000000000000000, -20.00000000000000000, 6.750000000004559908 ) ) ;
#17635 = EDGE_LOOP ( 'NONE', ( #9268, #12907 ) ) ;
#17636 = LINE ( 'NONE', #15842, #2763 ) ;
#17637 = PRODUCT_DEFINITION_SHAPE ( 'NONE', 'NONE',  #12504 ) ;
#17638 = ORIENTED_EDGE ( 'NONE', *, *, #8080, .T. ) ;
#17639 = FACE_OUTER_BOUND ( 'NONE', #18696, .T. ) ;
#17640 = LINE ( 'NONE', #15846, #13665 ) ;
#17641 = EDGE_LOOP ( 'NONE', ( #13339, #17569, #21356, #9536, #658, #22459 ) ) ;
#17642 = DIRECTION ( 'NONE',  ( -1.000000000000000000, -1.829748171496159792E-16, -1.829748171496159792E-16 ) ) ;
#17643 = EDGE_CURVE ( 'NONE', #18788, #12123, #3939, .T. ) ;
#17644 = ORIENTED_EDGE ( 'NONE', *, *, #5363, .T. ) ;
#17645 = DIRECTION ( 'NONE',  ( -0.9730401042858022320, 0.2306359803922080343, 5.959266323858941219E-17 ) ) ;
#17646 = SHAPE_REPRESENTATION ( 'F3', ( #12739 ), #19550 ) ;
#17647 = DATE_AND_TIME ( #1117, #9232 ) ;
#17648 = CARTESIAN_POINT ( 'NONE',  ( 31.49315201223960159, -2.613324229818170252, -13.00000000000039968 ) ) ;
#17649 = VECTOR ( 'NONE', #9047, 1000.000000000000114 ) ;
#17650 = APPROVAL ( #3773, 'UNKNOWN' ) ;
#17651 = CC_DESIGN_DATE_AND_TIME_ASSIGNMENT ( #3114, #12159, ( #6763 ) ) ;
#17652 = DATE_AND_TIME ( #21079, #9199 ) ;
#17653 =( NAMED_UNIT ( * ) SI_UNIT ( $, .STERADIAN. ) SOLID_ANGLE_UNIT ( ) );
#17654 = LINE ( 'NONE', #21081, #22112 ) ;
#17655 = EDGE_CURVE ( 'NONE', #7126, #554, #7724, .T. ) ;
#17656 = ADVANCED_FACE ( 'NONE', ( #21841 ), #19489, .T. ) ;
#17657 = CARTESIAN_POINT ( 'NONE',  ( -20.00000000397270128, 22.95208919256889857, 2.500000000000000000 ) ) ;
#17658 = SHAPE_REPRESENTATION_RELATIONSHIP ( 'NONE' , 'NONE' ,  #10092, #16427 ) ;
#17659 = DIRECTION ( 'NONE',  ( -2.982858504577319616E-17, 2.441916418604790135E-15, 1.000000000000000000 ) ) ;
#17660 = ORIENTED_EDGE ( 'NONE', *, *, #2945, .T. ) ;
#17661 = DIRECTION ( 'NONE',  ( -0.2306359803922053142, -0.9730401042858028982, 0.000000000000000000 ) ) ;
#17662 = VECTOR ( 'NONE', #8651, 1000.000000000000000 ) ;
#17663 = CARTESIAN_POINT ( 'NONE',  ( 105.8171986446039909, -20.23006919877430221, -13.00000000000000000 ) ) ;
#17664 = ORIENTED_EDGE ( 'NONE', *, *, #21250, .T. ) ;
#17665 = CARTESIAN_POINT ( 'NONE',  ( 34.27363088173783723, 8.178923185754959135, -8.806404184311304562 ) ) ;
#17666 = CARTESIAN_POINT ( 'NONE',  ( -20.18494928784681264, 20.45893982632658492, -4.999999999995553779 ) ) ;
#17667 = EDGE_LOOP ( 'NONE', ( #16008, #20856, #10224, #8818 ) ) ;
#17668 = CALENDAR_DATE ( 2026, 31, 10 ) ;
#17669 = FACE_OUTER_BOUND ( 'NONE', #4522, .T. ) ;
#17670 = ORIENTED_EDGE ( 'NONE', *, *, #7740, .F. ) ;
#17671 = ORIENTED_EDGE ( 'NONE', *, *, #5487, .T. ) ;
#17672 = COORDINATED_UNIVERSAL_TIME_OFFSET ( 0, 0, .AHEAD. ) ;
#17673 = CARTESIAN_POINT ( 'NONE',  ( 35.34171762861025456, 30.38879166913045182, -16.00000000000029843 ) ) ;
#17674 = EDGE_CURVE ( 'NONE', #22958, #15635, #3786, .T. ) ;
#17675 = ORIENTED_EDGE ( 'NONE', *, *, #6445, .F. ) ;
#17676 = CARTESIAN_POINT ( 'NONE',  ( 33.27705887009660302, -3.036156860536499913, 13.00000000000000000 ) ) ;
#17677 = COORDINATED_UNIVERSAL_TIME_OFFSET ( 0, 0, .AHEAD. ) ;
#17678 = CC_DESIGN_PERSON_AND_ORGANIZATION_ASSIGNMENT ( #16618, #20321, ( #11856 ) ) ;
#17679 = CC_DESIGN_PERSON_AND_ORGANIZATION_ASSIGNMENT ( #7044, #3548, ( #8383 ) ) ;
#17680 = APPROVAL_STATUS ( 'not_yet_approved' ) ;
#17681 = DIRECTION ( 'NONE',  ( -1.000000000000000000, -6.662112528310618598E-09, 2.269018306577664942E-13 ) ) ;
#17682 = EDGE_CURVE ( 'NONE', #5709, #16270, #3679, .T. ) ;
#17683 = EDGE_CURVE ( 'NONE', #5287, #16237, #23270, .T. ) ;
#17684 = AXIS2_PLACEMENT_3D ( 'NONE', #14133, #1522, #8790 ) ;
#17685 = FACE_OUTER_BOUND ( 'NONE', #21198, .T. ) ;
#17686 = EDGE_LOOP ( 'NONE', ( #19068, #22849, #4985, #8260 ) ) ;
#17687 = EDGE_LOOP ( 'NONE', ( #3981, #10445, #9499, #22116 ) ) ;
#17688 = CARTESIAN_POINT ( 'NONE',  ( 33.37436288052550992, -3.059220458576291435, 15.50000000000019895 ) ) ;
#17689 = CARTESIAN_POINT ( 'NONE',  ( 35.84667945578129888, -10.83917230622230043, -3.099999999999909939 ) ) ;
#17690 = ORIENTED_EDGE ( 'NONE', *, *, #6434, .F. ) ;
#17691 = CARTESIAN_POINT ( 'NONE',  ( 39.27359436029389883, 22.26288585089429972, -13.00000000000030020 ) ) ;
#17692 = DIRECTION ( 'NONE',  ( 0.000000000000000000, 0.000000000000000000, 1.000000000000000000 ) ) ;
#17693 = ORIENTED_EDGE ( 'NONE', *, *, #10859, .T. ) ;
#17694 = ORIENTED_EDGE ( 'NONE', *, *, #1127, .T. ) ;
#17695 = DIRECTION ( 'NONE',  ( -0.2306359803922053697, -0.9730401042858028982, 0.000000000000000000 ) ) ;
#17696 = ORIENTED_EDGE ( 'NONE', *, *, #18437, .T. ) ;
#17697 = APPROVAL_STATUS ( 'not_yet_approved' ) ;
#17698 = AXIS2_PLACEMENT_3D ( 'NONE', #18796, #9657, #13444 ) ;
#17699 = MANIFOLD_SOLID_BREP ( 'Imported1', #16624 ) ;
#17700 = EDGE_CURVE ( 'NONE', #11069, #16383, #20062, .T. ) ;
#17701 = ORIENTED_EDGE ( 'NONE', *, *, #12008, .F. ) ;
#17702 = EDGE_LOOP ( 'NONE', ( #11967, #23094, #22340, #21464 ) ) ;
#17703 = DIRECTION ( 'NONE',  ( 0.9730401042858036753, -0.2306359803922028995, -5.432877459303547669E-17 ) ) ;
#17704 = PERSON_AND_ORGANIZATION ( #11966, #8758 ) ;
#17705 = ADVANCED_FACE ( 'NONE', ( #3678 ), #5933, .T. ) ;
#17706 = CARTESIAN_POINT ( 'NONE',  ( 36.84099409957980242, 22.83947580187480142, 8.749999999999998224 ) ) ;
#17707 = EDGE_CURVE ( 'NONE', #13630, #16214, #9251, .T. ) ;
#17708 = AXIS2_PLACEMENT_3D ( 'NONE', #14628, #9655, #16744 ) ;
#17709 = EDGE_CURVE ( 'NONE', #22271, #20293, #16715, .T. ) ;
#17710 = AXIS2_PLACEMENT_3D ( 'NONE', #12063, #13704, #8361 ) ;
#17711 =( NAMED_UNIT ( * ) PLANE_ANGLE_UNIT ( ) SI_UNIT ( $, .RADIAN. ) );
#17712 = DIRECTION ( 'NONE',  ( 0.9730401042858036753, -0.2306359803922028995, -5.432877459303547669E-17 ) ) ;
#17713 = DATE_AND_TIME ( #5338, #4187 ) ;
#17714 = ORIENTED_EDGE ( 'NONE', *, *, #9558, .T. ) ;
#17715 = FACE_OUTER_BOUND ( 'NONE', #5940, .T. ) ;
#17716 = CARTESIAN_POINT ( 'NONE',  ( 39.74442752440959481, 5.605205456207790427, 20.00000000000000000 ) ) ;
#17717 = ORIENTED_EDGE ( 'NONE', *, *, #16451, .T. ) ;
#17718 = CARTESIAN_POINT ( 'NONE',  ( -21.99996573044222004, -0.1151926037937907599, -2.499999999999999556 ) ) ;
#17719 = DIRECTION ( 'NONE',  ( -2.270069654138865127E-15, -1.000000000000000000, -4.574083617919690056E-30 ) ) ;
#17720 = DIRECTION ( 'NONE',  ( 0.1187863113461966047, 0.5011527021216413136, -0.8571673007021102242 ) ) ;
#17721 = ORIENTED_EDGE ( 'NONE', *, *, #8356, .F. ) ;
#17722 = FACE_OUTER_BOUND ( 'NONE', #16830, .T. ) ;
#17723 = COORDINATED_UNIVERSAL_TIME_OFFSET ( 0, 0, .AHEAD. ) ;
#17724 = AXIS2_PLACEMENT_3D ( 'NONE', #22626, #13154, #17191 ) ;
#17725 = EDGE_LOOP ( 'NONE', ( #21607, #8559, #19527, #23255 ) ) ;
#17726 = ORIENTED_EDGE ( 'NONE', *, *, #22829, .F. ) ;
#17727 = DIRECTION ( 'NONE',  ( 8.911056267098788616E-18, 1.998401444326210262E-15, 1.000000000000000000 ) ) ;
#17728 = CARTESIAN_POINT ( 'NONE',  ( 117.1241794131700118, -12.63305097454430026, 15.90000000000000036 ) ) ;
#17729 = AXIS2_PLACEMENT_3D ( 'NONE', #8139, #23064, #22950 ) ;
#17730 = DIRECTION ( 'NONE',  ( 1.000000000000000000, 0.000000000000000000, 0.000000000000000000 ) ) ;
#17731 = PERSON_AND_ORGANIZATION ( #11966, #8758 ) ;
#17732 = PRODUCT_RELATED_PRODUCT_CATEGORY ( 'detail', '', ( #19526 ) ) ;
#17733 = CARTESIAN_POINT ( 'NONE',  ( -16.50058068176721804, 23.02794805996685668, 3.749999999999900080 ) ) ;
#17734 = DIRECTION ( 'NONE',  ( 0.9730401042858036753, -0.2306359803922031493, 2.804983810440361760E-16 ) ) ;
#17735 = CIRCLE ( 'NONE', #13182, 4.250000000000000000 ) ;
#17736 = DIRECTION ( 'NONE',  ( 1.000000000000000000, 0.000000000000000000, 0.000000000000000000 ) ) ;
#17737 = AXIS2_PLACEMENT_3D ( 'NONE', #21149, #4656, #11931 ) ;
#17739 = LINE ( 'NONE', #5029, #8677 ) ;
#17738 = AXIS2_PLACEMENT_3D ( 'NONE', #13967, #3165, #8393 ) ;
#17740 = PERSON_AND_ORGANIZATION_ROLE ( 'design_supplier' ) ;
#17741 = AXIS2_PLACEMENT_3D ( 'NONE', #21313, #21433, #19767 ) ;
#17742 = AXIS2_PLACEMENT_3D ( 'NONE', #16265, #9550, #1888 ) ;
#17743 = LINE ( 'NONE', #20939, #21610 ) ;
#17744 = CARTESIAN_POINT ( 'NONE',  ( 33.90884364377009774, 10.17428291754599989, -27.69000000000049866 ) ) ;
#17745 = FACE_OUTER_BOUND ( 'NONE', #17725, .T. ) ;
#17746 = ADVANCED_FACE ( 'NONE', ( #14720, #3924 ), #4151, .T. ) ;
#17747 = CARTESIAN_POINT ( 'NONE',  ( -17.47493720815199936, 28.95208920939580111, 5.500000000004419576 ) ) ;
#17748 = DIRECTION ( 'NONE',  ( 1.000000000000000000, -1.466984912809909902E-16, 5.345529420184390105E-52 ) ) ;
#17749 = EDGE_LOOP ( 'NONE', ( #2238, #13943 ) ) ;
#17750 = DIRECTION ( 'NONE',  ( 0.000000000000000000, 0.000000000000000000, -1.000000000000000000 ) ) ;
#17751 = ORIENTED_EDGE ( 'NONE', *, *, #15908, .F. ) ;
#17752 = DIRECTION ( 'NONE',  ( 0.9822637906114334294, -0.1875042550281410536, 4.933538860811975815E-16 ) ) ;
#17753 = DIRECTION ( 'NONE',  ( -2.982858504577319616E-17, 2.441916418604790135E-15, 1.000000000000000000 ) ) ;
#17754 = AXIS2_PLACEMENT_3D ( 'NONE', #8579, #2981, #8690 ) ;
#17755 = VERTEX_POINT ( 'NONE', #16856 ) ;
#17756 = CARTESIAN_POINT ( 'NONE',  ( 32.67740532107718820, -5.566061131680170249, 13.00000000000019895 ) ) ;
#17757 = CONICAL_SURFACE ( 'NONE', #7513, 1.033499999999998753, 1.029744258676650093 ) ;
#17758 = EDGE_LOOP ( 'NONE', ( #4326, #7207, #21397, #6292 ) ) ;
#17759 = CARTESIAN_POINT ( 'NONE',  ( 115.3944095602285387, -19.93085175668762332, -13.00000000000000000 ) ) ;
#17760 = APPLICATION_PROTOCOL_DEFINITION ( 'international standard', 'config_control_design', 1994, #7460 ) ;
#17761 = DIRECTION ( 'NONE',  ( -0.2306359803922101437, -0.9730401042858018990, 4.373252460445732608E-15 ) ) ;
#17762 = DIRECTION ( 'NONE',  ( -6.123230174520380038E-17, -4.962644601432260272E-15, -1.000000000000000000 ) ) ;
#17763 = CARTESIAN_POINT ( 'NONE',  ( -19.99975861755300244, 22.95209442650120124, 3.749999999999900080 ) ) ;
#17764 = DIRECTION ( 'NONE',  ( 0.000000000000000000, 0.000000000000000000, 1.000000000000000000 ) ) ;
#17765 = CIRCLE ( 'NONE', #20774, 6.000000000001507239 ) ;
#17766 = FACE_OUTER_BOUND ( 'NONE', #8751, .T. ) ;
#17767 = EDGE_LOOP ( 'NONE', ( #4700, #7527, #9276 ) ) ;
#17768 = FACE_OUTER_BOUND ( 'NONE', #9652, .T. ) ;
#17769 = EDGE_CURVE ( 'NONE', #15538, #13655, #7375, .T. ) ;
#17770 = DESIGN_CONTEXT ( 'detailed design', #23228, 'design' ) ;
#17771 = SPHERICAL_SURFACE ( 'NONE', #19395, 8.000000000000000000 ) ;
#17772 = ORIENTED_EDGE ( 'NONE', *, *, #21301, .F. ) ;
#17773 = CARTESIAN_POINT ( 'NONE',  ( 117.1933702072879981, -12.34113894325849969, 19.59999999999999787 ) ) ;
#17774 = CC_DESIGN_PERSON_AND_ORGANIZATION_ASSIGNMENT ( #1014, #11524, ( #22778 ) ) ;
#17775 = ORIENTED_EDGE ( 'NONE', *, *, #16798, .F. ) ;
#17776 = ITEM_DEFINED_TRANSFORMATION ( 'NONE', 'NONE', #18423,  #12739 ) ;
#17777 = PLANE ( 'NONE',  #11926 ) ;
#17778 =( BOUNDED_CURVE ( )  B_SPLINE_CURVE ( 2, ( #21980, #3602, #21634 ),
 .UNSPECIFIED., .F., .F. ) 
 B_SPLINE_CURVE_WITH_KNOTS ( ( 3, 3 ),
 ( 0.000000000000000000, 0.5842180690389598974 ),
 .UNSPECIFIED. ) 
 CURVE ( )  GEOMETRIC_REPRESENTATION_ITEM ( )  RATIONAL_B_SPLINE_CURVE ( ( 1.000000000000000000, 1.154700538379249908, 1.000000000000000000 ) ) 
 REPRESENTATION_ITEM ( '' )  );
#17779 = ORIENTED_EDGE ( 'NONE', *, *, #13459, .T. ) ;
#17780 = ORIENTED_EDGE ( 'NONE', *, *, #16966, .F. ) ;
#17781 = EDGE_CURVE ( 'NONE', #19301, #3524, #15713, .T. ) ;
#17782 = ADVANCED_FACE ( 'NONE', ( #7959 ), #9863, .T. ) ;
#17783 = PERSON_AND_ORGANIZATION ( #11966, #8758 ) ;
#17784 = CARTESIAN_POINT ( 'NONE',  ( 36.30836311812279860, 20.59233593730800038, 13.00000000000000000 ) ) ;
#17785 = VERTEX_POINT ( 'NONE', #9755 ) ;
#17786 = DIRECTION ( 'NONE',  ( -0.9730401042858036753, 0.2306359803922028995, 5.958148513035547083E-17 ) ) ;
#17787 = CALENDAR_DATE ( 2026, 31, 10 ) ;
#17788 = CLOSED_SHELL ( 'NONE', ( #8083, #23048, #20749, #17478, #13865, #4878, #11470, #2711, #7402, #20843, #9261, #7541, #2369, #12295, #3904, #21469, #2291, #13729, #926, #5305, #12587, #18134, #16246, #7957, #4450, #20265, #4451, #10149, #22152, #10265, #14047, #4539, #20964, #9936, #21239, #20965, #15163, #16528, #20055, #22134, #7795, #22460, #3172, #64, #6454, #23315, #22415, #4333, #117, #15942, #13158, #5796, #11160, #770, #20797, #19341, #972, #11764, #7574, #14792, #16028, #11478, #1711, #976, #20559, #12278, #1470, #3027, #10394, #7162, #7287, #22751, #19596, #15510, #7361, #2987, #2640, #4346, #21448, #22395, #20656, #3197, #13609, #9059, #17705, #4541, #22494, #7611, #5565, #18555, #14146, #15231, #22791, #846, #20700, #4550, #21802, #4022, #8223, #18527, #20984, #13277, #1438, #4586, #12806, #22612, #21145, #11523, #2266, #13688, #20275 ) ) ;
#17789 = ITEM_DEFINED_TRANSFORMATION ( 'NONE', 'NONE', #19715,  #12739 ) ;
#17790 = DIRECTION ( 'NONE',  ( -1.000000000000000000, -9.248855984704951398E-11, 1.138590270700269951E-14 ) ) ;
#17791 = DIRECTION ( 'NONE',  ( 0.000000000000000000, 0.000000000000000000, 1.000000000000000000 ) ) ;
#17792 = AXIS2_PLACEMENT_3D ( 'NONE', #17287, #7788, #15258 ) ;
#17793 = ORIENTED_EDGE ( 'NONE', *, *, #21702, .T. ) ;
#17794 = ADVANCED_FACE ( 'NONE', ( #17091 ), #13646, .F. ) ;
#17795 = ORIENTED_EDGE ( 'NONE', *, *, #7331, .T. ) ;
#17796 = CARTESIAN_POINT ( 'NONE',  ( 34.89491389100820129, 23.30074776265919922, 13.00000000000000000 ) ) ;
#17797 = CARTESIAN_POINT ( 'NONE',  ( -25.49859074735509878, -0.2321374729090499855, 3.750000000000000000 ) ) ;
#17798 = ORIENTED_EDGE ( 'NONE', *, *, #12845, .T. ) ;
#17799 = CC_DESIGN_PERSON_AND_ORGANIZATION_ASSIGNMENT ( #12083, #15499, ( #15292 ) ) ;
#17800 = EDGE_CURVE ( 'NONE', #2277, #1222, #8892, .T. ) ;
#17801 = CC_DESIGN_PERSON_AND_ORGANIZATION_ASSIGNMENT ( #7127, #19699, ( #4578 ) ) ;
#17802 = CARTESIAN_POINT ( 'NONE',  ( -19.99975861755300244, 22.95209442650120124, 2.499999999999900524 ) ) ;
#17803 = FACE_OUTER_BOUND ( 'NONE', #18660, .T. ) ;
#17804 = VERTEX_POINT ( 'NONE', #13775 ) ;
#17805 = ORIENTED_EDGE ( 'NONE', *, *, #21080, .F. ) ;
#17806 = EDGE_CURVE ( 'NONE', #11097, #11763, #18411, .T. ) ;
#17807 = EDGE_CURVE ( 'NONE', #19697, #227, #5090, .T. ) ;
#17808 = APPROVAL_DATE_TIME ( #10582, #6483 ) ;
#17809 = ORIENTED_EDGE ( 'NONE', *, *, #7445, .F. ) ;
#17810 = ORIENTED_EDGE ( 'NONE', *, *, #4288, .T. ) ;
#17811 = APPROVAL ( #11194, 'UNSPECIFIED' ) ;
#17812 = DIRECTION ( 'NONE',  ( -5.944927207247209745E-47, -1.000000000000000000, 0.000000000000000000 ) ) ;
#17813 = LOCAL_TIME ( 14, 11, 27.00000000000000000, #21591 ) ;
#17814 = CALENDAR_DATE ( 2026, 31, 10 ) ;
#17815 = VECTOR ( 'NONE', #3488, 1000.000000000000114 ) ;
#17816 = CARTESIAN_POINT ( 'NONE',  ( -20.00000000000000000, -20.00000000000000000, -4.999999999995470290 ) ) ;
#17817 = DIRECTION ( 'NONE',  ( -1.138590270679730064E-14, -2.220446049251235259E-15, -1.000000000000000000 ) ) ;
#17818 = APPLICATION_PROTOCOL_DEFINITION ( 'international standard', 'config_control_design', 1994, #21248 ) ;
#17819 = ADVANCED_FACE ( 'NONE', ( #4503 ), #22546, .F. ) ;
#17820 = PRODUCT_DEFINITION_SHAPE ( 'NONE', 'NONE',  #19247 ) ;
#17821 = VERTEX_POINT ( 'NONE', #2729 ) ;
#17822 = CIRCLE ( 'NONE', #18594, 2.499999999999998668 ) ;
#17823 = CARTESIAN_POINT ( 'NONE',  ( 34.67470932959370344, 24.53963568513860238, -11.00000000000049916 ) ) ;
#17824 = VECTOR ( 'NONE', #20777, 1000.000000000000000 ) ;
#17825 = DIRECTION ( 'NONE',  ( 1.000000000000000000, 0.000000000000000000, 0.000000000000000000 ) ) ;
#17826 = ORIENTED_EDGE ( 'NONE', *, *, #350, .F. ) ;
#17827 = ADVANCED_FACE ( 'NONE', ( #17336 ), #20539, .F. ) ;
#17828 = CARTESIAN_POINT ( 'NONE',  ( -20.00000000000000000, -20.00000000000000000, 5.000000000004559908 ) ) ;
#17829 = DIRECTION ( 'NONE',  ( 0.1630842657209334579, 0.6880432561069538266, -0.7071067811865507924 ) ) ;
#17830 = DIRECTION ( 'NONE',  ( 0.000000000000000000, 0.000000000000000000, 1.000000000000000000 ) ) ;
#17831 = VERTEX_POINT ( 'NONE', #19231 ) ;
#17832 = ORIENTED_EDGE ( 'NONE', *, *, #13236, .T. ) ;
#17833 = DIRECTION ( 'NONE',  ( -6.662112528310618598E-09, 1.000000000000000000, -2.081668171172169697E-15 ) ) ;
#17834 = EDGE_CURVE ( 'NONE', #18753, #7665, #21380, .T. ) ;
#17835 = PERSON_AND_ORGANIZATION ( #11966, #8758 ) ;
#17837 = EDGE_CURVE ( 'NONE', #10039, #10837, #14943, .T. ) ;
#17836 = VERTEX_POINT ( 'NONE', #11772 ) ;
#17838 = EDGE_LOOP ( 'NONE', ( #11430, #2637, #17924, #14520, #17896 ) ) ;
#17839 = DIRECTION ( 'NONE',  ( 0.2306359803922031215, 0.9730401042858035643, -4.741332172907962143E-18 ) ) ;
#17840 = DIRECTION ( 'NONE',  ( -0.9730401042858035643, 0.2306359803922028717, 6.126766849694256332E-17 ) ) ;
#17841 = DIRECTION ( 'NONE',  ( 0.000000000000000000, 0.000000000000000000, -1.000000000000000000 ) ) ;
#17842 = CALENDAR_DATE ( 2026, 31, 10 ) ;
#17843 = CARTESIAN_POINT ( 'NONE',  ( -69.88753305544580030, 2.884110939634079607, 5.500000000000099476 ) ) ;
#17844 = CC_DESIGN_SECURITY_CLASSIFICATION ( #19033, ( #16680 ) ) ;
#17845 = CARTESIAN_POINT ( 'NONE',  ( 44.09191575480142689, 23.94701142199386368, 12.99999999999970512 ) ) ;
#17846 = AXIS2_PLACEMENT_3D ( 'NONE', #749, #534, #11725 ) ;
#17847 = DIRECTION ( 'NONE',  ( 0.000000000000000000, 0.000000000000000000, 1.000000000000000000 ) ) ;
#17848 = ORIENTED_EDGE ( 'NONE', *, *, #17496, .T. ) ;
#17849 = CYLINDRICAL_SURFACE ( 'NONE', #22298, 4.349999999999996980 ) ;
#17850 = PERSON_AND_ORGANIZATION ( #11966, #8758 ) ;
#17851 = VECTOR ( 'NONE', #10970, 1000.000000000000114 ) ;
#17852 = CARTESIAN_POINT ( 'NONE',  ( -19.99999999999809930, -20.00000000000000000, 8.250000000004551026 ) ) ;
#17853 = FACE_OUTER_BOUND ( 'NONE', #3036, .T. ) ;
#17854 = DIRECTION ( 'NONE',  ( -0.2306359803922028717, -0.9730401042858035643, -4.801075795095373112E-17 ) ) ;
#17855 = LOCAL_TIME ( 14, 11, 27.00000000000000000, #11936 ) ;
#17856 = DIRECTION ( 'NONE',  ( -0.9730401042858022320, 0.2306359803922080343, 5.959266323858941219E-17 ) ) ;
#17857 = ADVANCED_FACE ( 'NONE', ( #810 ), #8084, .T. ) ;
#17858 = CARTESIAN_POINT ( 'NONE',  ( 40.21613903755275743, 8.679288774590558475, 26.88000000000000611 ) ) ;
#17859 = CC_DESIGN_APPROVAL ( #2920, ( #11812 ) ) ;
#17860 = ORIENTED_EDGE ( 'NONE', *, *, #18810, .F. ) ;
#17861 = CARTESIAN_POINT ( 'NONE',  ( 33.77054299527826942, 10.75717911589417319, 8.985048276826017144 ) ) ;
#17862 = VERTEX_POINT ( 'NONE', #8307 ) ;
#17863 = LINE ( 'NONE', #5383, #14907 ) ;
#17864 = CARTESIAN_POINT ( 'NONE',  ( 37.46113131852679601, -4.027891576221660053, 13.00000000000000000 ) ) ;
#17865 = EDGE_LOOP ( 'NONE', ( #2687, #3399, #10731, #8405 ) ) ;
#17866 = AXIS2_PLACEMENT_3D ( 'NONE', #9603, #23088, #14083 ) ;
#17867 = DIRECTION ( 'NONE',  ( 1.749697687229200179E-14, 7.407713590345340554E-14, -1.000000000000000000 ) ) ;
#17868 = ADVANCED_BREP_SHAPE_REPRESENTATION ( '', ( #9489, #12739 ), #743 ) ;
#17869 = ORIENTED_EDGE ( 'NONE', *, *, #2822, .F. ) ;
#17870 = PERSON_AND_ORGANIZATION ( #11966, #8758 ) ;
#17871 = DIRECTION ( 'NONE',  ( 0.000000000000000000, 0.000000000000000000, -1.000000000000000000 ) ) ;
#17872 = EDGE_CURVE ( 'NONE', #10146, #17804, #521, .T. ) ;
#17873 = LOCAL_TIME ( 14, 11, 27.00000000000000000, #339 ) ;
#17874 = CC_DESIGN_SECURITY_CLASSIFICATION ( #9917, ( #3463 ) ) ;
#17875 = FACE_OUTER_BOUND ( 'NONE', #25, .T. ) ;
#17876 = CYLINDRICAL_SURFACE ( 'NONE', #15087, 0.3999999999999982458 ) ;
#17877 = DIRECTION ( 'NONE',  ( 1.000000000000000000, 0.000000000000000000, 0.000000000000000000 ) ) ;
#17878 = SECURITY_CLASSIFICATION ( '', '', #12101 ) ;
#17879 = LOCAL_TIME ( 14, 11, 27.00000000000000000, #21917 ) ;
#17880 = FACE_OUTER_BOUND ( 'NONE', #9457, .T. ) ;
#17881 = DIRECTION ( 'NONE',  ( -0.07397971354964476276, -0.9972597464969256142, 2.428612866367529538E-15 ) ) ;
#17882 = DIRECTION ( 'NONE',  ( -0.9999862922474491711, -0.005235963827128305680, 1.187304881134278487E-16 ) ) ;
#17883 = DIRECTION ( 'NONE',  ( -0.2306359803922076734, -0.9730401042858024541, 1.412237191019896754E-17 ) ) ;
#17884 = ORIENTED_EDGE ( 'NONE', *, *, #11833, .T. ) ;
#17885 = LINE ( 'NONE', #19905, #5065 ) ;
#17886 = CARTESIAN_POINT ( 'NONE',  ( 34.67470932959380292, 24.53963568513870186, 15.00000000000000000 ) ) ;
#17887 = ORIENTED_EDGE ( 'NONE', *, *, #4769, .F. ) ;
#17888 = LOCAL_TIME ( 14, 11, 27.00000000000000000, #19914 ) ;
#17889 = CARTESIAN_POINT ( 'NONE',  ( -26.99999999999959854, -30.09999999999999787, 23.00000000000000000 ) ) ;
#17890 = VERTEX_POINT ( 'NONE', #4743 ) ;
#17891 = VERTEX_POINT ( 'NONE', #15541 ) ;
#17892 = CIRCLE ( 'NONE', #21670, 2.066999999999998394 ) ;
#17893 = VECTOR ( 'NONE', #5244, 1000.000000000000000 ) ;
#17894 = PERSON_AND_ORGANIZATION_ROLE ( 'design_supplier' ) ;
#17895 = CARTESIAN_POINT ( 'NONE',  ( 1.358598381910800010E-16, -1.434096706618689895E-15, 8.874009851233079243E-14 ) ) ;
#17896 = ORIENTED_EDGE ( 'NONE', *, *, #9828, .F. ) ;
#17897 = DIRECTION ( 'NONE',  ( 3.099353312215989243E-62, 1.872670541876879671E-92, -1.000000000000000000 ) ) ;
#17898 = LOCAL_TIME ( 14, 11, 27.00000000000000000, #13034 ) ;
#17899 = COORDINATED_UNIVERSAL_TIME_OFFSET ( 0, 0, .AHEAD. ) ;
#17900 = EDGE_CURVE ( 'NONE', #16644, #23121, #17230, .T. ) ;
#17901 = EDGE_CURVE ( 'NONE', #9054, #104, #10221, .T. ) ;
#17902 = COORDINATED_UNIVERSAL_TIME_OFFSET ( 0, 0, .AHEAD. ) ;
#17903 = CARTESIAN_POINT ( 'NONE',  ( 39.37089837072280574, 22.23982225285502068, -15.50000000000049916 ) ) ;
#17904 = LOCAL_TIME ( 14, 11, 27.00000000000000000, #18552 ) ;
#17905 = CARTESIAN_POINT ( 'NONE',  ( 2.500000000000000000, -17.30000000000000071, -5.000000000000000000 ) ) ;
#17906 = AXIS2_PLACEMENT_3D ( 'NONE', #17634, #19523, #10514 ) ;
#17907 = VERTEX_POINT ( 'NONE', #22308 ) ;
#17908 = DIRECTION ( 'NONE',  ( 0.9999862922474493931, 0.005235963827117055998, -1.750845403988397166E-31 ) ) ;
#17909 = EDGE_CURVE ( 'NONE', #21550, #23097, #6616, .T. ) ;
#17910 = EDGE_CURVE ( 'NONE', #8641, #20176, #9658, .T. ) ;
#17911 = CIRCLE ( 'NONE', #14504, 5.000000000000002665 ) ;
#17912 = CIRCLE ( 'NONE', #9584, 2.499999999999999556 ) ;
#17913 = ORIENTED_EDGE ( 'NONE', *, *, #7347, .F. ) ;
#17914 =( BOUNDED_CURVE ( )  B_SPLINE_CURVE ( 2, ( #12096, #3039, #10310 ),
 .UNSPECIFIED., .F., .F. ) 
 B_SPLINE_CURVE_WITH_KNOTS ( ( 3, 3 ),
 ( 0.1168436138077924430, 0.2336872276155859962 ),
 .UNSPECIFIED. ) 
 CURVE ( )  GEOMETRIC_REPRESENTATION_ITEM ( )  RATIONAL_B_SPLINE_CURVE ( ( 1.077350269189625065, 1.077350269189625287, 1.000000000000000000 ) ) 
 REPRESENTATION_ITEM ( '' )  );
#17915 = SECURITY_CLASSIFICATION ( '', '', #2823 ) ;
#17916 = LINE ( 'NONE', #8900, #22811 ) ;
#17917 = CARTESIAN_POINT ( 'NONE',  ( 65.59135885879943828, 15.51103319044781870, 1.043520735224289159E-14 ) ) ;
#17918 = ORIENTED_EDGE ( 'NONE', *, *, #4633, .F. ) ;
#17919 = CIRCLE ( 'NONE', #9590, 2.500000000000000444 ) ;
#17920 = AXIS2_PLACEMENT_3D ( 'NONE', #7608, #11324, #20667 ) ;
#17921 = DIRECTION ( 'NONE',  ( -0.7071067811865475727, 1.387778780781445281E-15, 0.7071067811865475727 ) ) ;
#17922 = ADVANCED_FACE ( 'NONE', ( #15672 ), #1286, .T. ) ;
#17923 = LINE ( 'NONE', #7014, #19842 ) ;
#17924 = ORIENTED_EDGE ( 'NONE', *, *, #7511, .T. ) ;
#17925 = ORIENTED_EDGE ( 'NONE', *, *, #10875, .F. ) ;
#17926 = PERSON_AND_ORGANIZATION_ROLE ( 'creator' ) ;
#17927 = SECURITY_CLASSIFICATION ( '', '', #7583 ) ;
#17928 = VERTEX_POINT ( 'NONE', #12465 ) ;
#17929 = ORIENTED_EDGE ( 'NONE', *, *, #21461, .T. ) ;
#17930 = FACE_OUTER_BOUND ( 'NONE', #10762, .T. ) ;
#17931 = PERSON_AND_ORGANIZATION_ROLE ( 'design_owner' ) ;
#17932 = VECTOR ( 'NONE', #15811, 1000.000000000000114 ) ;
#17933 = VECTOR ( 'NONE', #9096, 1000.000000000000114 ) ;
#17934 = EDGE_CURVE ( 'NONE', #16466, #1142, #14199, .T. ) ;
#17935 = AXIS2_PLACEMENT_3D ( 'NONE', #8754, #23231, #5185 ) ;
#17936 = DIRECTION ( 'NONE',  ( 0.9730401042858036753, -0.2306359803922028995, -5.432877459303547669E-17 ) ) ;
#17937 = DATE_AND_TIME ( #7023, #6051 ) ;
#17938 = APPLICATION_CONTEXT ( 'configuration controlled 3d designs of mechanical parts and assemblies' ) ;
#17939 = CC_DESIGN_PERSON_AND_ORGANIZATION_ASSIGNMENT ( #6036, #6391, ( #6812 ) ) ;
#17940 = AXIS2_PLACEMENT_3D ( 'NONE', #8718, #20946, #6953 ) ;
#17941 = APPROVAL ( #9681, 'UNSPECIFIED' ) ;
#17942 =( NAMED_UNIT ( * ) SI_UNIT ( $, .STERADIAN. ) SOLID_ANGLE_UNIT ( ) );
#17943 = CARTESIAN_POINT ( 'NONE',  ( 34.40556712239440174, 8.514986143070949254, -27.69000000000049866 ) ) ;
#17944 = AXIS2_PLACEMENT_3D ( 'NONE', #10679, #17791, #12232 ) ;
#17945 = EDGE_CURVE ( 'NONE', #19198, #2339, #19695, .T. ) ;
#17946 = EDGE_CURVE ( 'NONE', #15927, #6737, #3953, .T. ) ;
#17947 = PERSON_AND_ORGANIZATION_ROLE ( 'design_supplier' ) ;
#17948 = PRODUCT_DEFINITION_FORMATION_WITH_SPECIFIED_SOURCE ( 'ANY', '', #17082, .NOT_KNOWN. ) ;
#17949 = ORIENTED_EDGE ( 'NONE', *, *, #16029, .T. ) ;
#17950 = DIRECTION ( 'NONE',  ( 0.9730401042858035643, -0.2306359803922028717, -5.958148513035547083E-17 ) ) ;
#17951 = AXIS2_PLACEMENT_3D ( 'NONE', #19471, #10578, #1636 ) ;
#17952 = CARTESIAN_POINT ( 'NONE',  ( -19.99999999999809930, -20.00000000000000000, 8.250000000004551026 ) ) ;
#17953 = ORIENTED_EDGE ( 'NONE', *, *, #6730, .T. ) ;
#17954 = CIRCLE ( 'NONE', #11907, 0.4000000000000010214 ) ;
#17955 = CARTESIAN_POINT ( 'NONE',  ( -19.99975861755300244, 22.95209442650120124, 4.999999999999900524 ) ) ;
#17956 = AXIS2_PLACEMENT_3D ( 'NONE', #2060, #5509, #17996 ) ;
#17957 = FACE_OUTER_BOUND ( 'NONE', #15463, .T. ) ;
#17958 = CARTESIAN_POINT ( 'NONE',  ( 44.03425675970473208, 23.70375139592372449, -13.00000000000000000 ) ) ;
#17959 = VERTEX_POINT ( 'NONE', #10465 ) ;
#17960 = VERTEX_POINT ( 'NONE', #13885 ) ;
#17961 = CARTESIAN_POINT ( 'NONE',  ( -3.458317987535629801, 19.03127855354509990, -7.892745253163399067E-16 ) ) ;
#17962 = ORIENTED_EDGE ( 'NONE', *, *, #15657, .F. ) ;
#17963 = PERSON_AND_ORGANIZATION ( #11966, #8758 ) ;
#17964 = ORIENTED_EDGE ( 'NONE', *, *, #17372, .T. ) ;
#17965 = VERTEX_POINT ( 'NONE', #3418 ) ;
#17966 = LINE ( 'NONE', #9480, #17210 ) ;
#17967 = FACE_BOUND ( 'NONE', #13638, .T. ) ;
#17968 = FACE_OUTER_BOUND ( 'NONE', #9305, .T. ) ;
#17969 = CALENDAR_DATE ( 2026, 31, 10 ) ;
#17970 = DIRECTION ( 'NONE',  ( 1.000000000000000000, -1.751019220569989865E-16, -7.006492321624090605E-47 ) ) ;
#17971 = EDGE_CURVE ( 'NONE', #131, #8021, #10342, .T. ) ;
#17972 = LOCAL_TIME ( 14, 11, 27.00000000000000000, #7422 ) ;
#17973 = VECTOR ( 'NONE', #8158, 999.9999999999998863 ) ;
#17974 = LINE ( 'NONE', #6697, #1525 ) ;
#17975 = VECTOR ( 'NONE', #23333, 1000.000000000000227 ) ;
#17976 = AXIS2_PLACEMENT_3D ( 'NONE', #13398, #13508, #13625 ) ;
#17977 = DIRECTION ( 'NONE',  ( 0.000000000000000000, 0.000000000000000000, 1.000000000000000000 ) ) ;
#17978 = EDGE_CURVE ( 'NONE', #9873, #16805, #19343, .T. ) ;
#17979 = ADVANCED_FACE ( 'NONE', ( #12242 ), #11193, .T. ) ;
#17980 = ORIENTED_EDGE ( 'NONE', *, *, #12685, .F. ) ;
#17981 = CARTESIAN_POINT ( 'NONE',  ( 43.98050001724080005, -5.573152644851309567, 13.00000000000019895 ) ) ;
#17982 = DATE_TIME_ROLE ( 'creation_date' ) ;
#17983 = DIRECTION ( 'NONE',  ( -6.123237831918399306E-17, 1.569224110909209817E-30, 1.000000000000000000 ) ) ;
#17984 = CARTESIAN_POINT ( 'NONE',  ( 114.2412296582679971, -24.79605227811670076, -2.999999999999940048 ) ) ;
#17985 = PLANE ( 'NONE',  #23360 ) ;
#17986 = AXIS2_PLACEMENT_3D ( 'NONE', #10652, #1596, #8871 ) ;
#17987 = CARTESIAN_POINT ( 'NONE',  ( -25.01253141238650102, 26.70208918381559826, 8.000000000004510170 ) ) ;
#17988 = DIRECTION ( 'NONE',  ( -6.281952996264309889E-17, -4.969341027148640384E-15, -1.000000000000000000 ) ) ;
#17989 = ORIENTED_EDGE ( 'NONE', *, *, #21394, .F. ) ;
#17990 = FACE_OUTER_BOUND ( 'NONE', #7015, .T. ) ;
#17991 = UNCERTAINTY_MEASURE_WITH_UNIT (LENGTH_MEASURE( 1.000000000000000082E-05 ), #3210, 'distance_accuracy_value', 'NONE');
#17992 = VERTEX_POINT ( 'NONE', #8429 ) ;
#17993 = CARTESIAN_POINT ( 'NONE',  ( 33.37436288052550282, -3.059220458576433099, -10.50000000000039968 ) ) ;
#17994 = DIRECTION ( 'NONE',  ( -9.594916218540590128E-33, 2.583840697242805182E-16, -1.000000000000000000 ) ) ;
#17995 = VERTEX_POINT ( 'NONE', #6771 ) ;
#17996 = DIRECTION ( 'NONE',  ( 0.2306359803922032325, 0.9730401042858035643, -1.407521210652540462E-17 ) ) ;
#17998 = VERTEX_POINT ( 'NONE', #19470 ) ;
#17997 = EDGE_CURVE ( 'NONE', #11146, #23127, #12323, .T. ) ;
#17999 = CARTESIAN_POINT ( 'NONE',  ( 36.88454136754629076, -6.460491836936111731, 13.00000000000000000 ) ) ;
#18000 = DATE_AND_TIME ( #10528, #21347 ) ;
#18001 = FACE_OUTER_BOUND ( 'NONE', #23343, .T. ) ;
#18002 = ADVANCED_FACE ( 'NONE', ( #12581, #14234 ), #21363, .F. ) ;
#18003 = DIRECTION ( 'NONE',  ( 0.000000000000000000, -5.527220191599521464E-16, -1.000000000000000000 ) ) ;
#18004 = ADVANCED_FACE ( 'NONE', ( #8904 ), #21472, .T. ) ;
#18005 = CARTESIAN_POINT ( 'NONE',  ( -11.72915887396500167, 20.99168438687879856, -3.119098571846229552E-15 ) ) ;
#18006 = EDGE_CURVE ( 'NONE', #20045, #6885, #17245, .T. ) ;
#18007 = CARTESIAN_POINT ( 'NONE',  ( -17.25000000397428934, 22.95208919256900160, -8.499999999996171951 ) ) ;
#18008 = CARTESIAN_POINT ( 'NONE',  ( -16.50000000144730095, -4.350228928666989958, 8.000000000004488854 ) ) ;
#18009 = FACE_OUTER_BOUND ( 'NONE', #7393, .T. ) ;
#18010 = DESIGN_CONTEXT ( 'detailed design', #22640, 'design' ) ;
#18011 = DIRECTION ( 'NONE',  ( 0.8633955506089472376, 0.5045276238112963441, 2.968109478347069028E-19 ) ) ;
#18012 = ORIENTED_EDGE ( 'NONE', *, *, #9691, .F. ) ;
#18013 = DIRECTION ( 'NONE',  ( 0.000000000000000000, -1.000000000000000000, 4.969341027244109908E-15 ) ) ;
#18014 = DIRECTION ( 'NONE',  ( 2.269747459788994803E-13, 2.220446049250480319E-15, 1.000000000000000000 ) ) ;
#18015 = ORIENTED_EDGE ( 'NONE', *, *, #20071, .T. ) ;
#18016 = CARTESIAN_POINT ( 'NONE',  ( -32.64674982798959491, 7.329300507370470008, 2.500000000000000000 ) ) ;
#18017 = EDGE_LOOP ( 'NONE', ( #3368, #5724 ) ) ;
#18018 = VECTOR ( 'NONE', #12625, 1000.000000000000114 ) ;
#18019 = DATE_AND_TIME ( #12678, #9156 ) ;
#18020 = CYLINDRICAL_SURFACE ( 'NONE', #824, 2.066999999999999726 ) ;
#18021 = ORIENTED_EDGE ( 'NONE', *, *, #21995, .T. ) ;
#18022 = DIRECTION ( 'NONE',  ( 3.210834492181045054E-17, -2.441916418604790135E-15, -1.000000000000000000 ) ) ;
#18023 = APPROVAL_ROLE ( '' ) ;
#18024 = APPROVAL ( #4439, 'UNSPECIFIED' ) ;
#18025 = PRODUCT_DEFINITION_SHAPE ( 'NONE', 'NONE',  #6840 ) ;
#18026 = ITEM_DEFINED_TRANSFORMATION ( 'NONE', 'NONE', #5537,  #12739 ) ;
#18027 = DIRECTION ( 'NONE',  ( 0.2306359803922087282, 0.9730401042858021210, 2.478176394252581732E-15 ) ) ;
#18028 = AXIS2_PLACEMENT_3D ( 'NONE', #9491, #5922, #6037 ) ;
#18029 = CARTESIAN_POINT ( 'NONE',  ( 28.14554285793940025, -3.006546890859610244, -15.00000000000039968 ) ) ;
#18030 = ORIENTED_EDGE ( 'NONE', *, *, #15063, .T. ) ;
#18031 = LINE ( 'NONE', #11166, #14743 ) ;
#18032 = ORIENTED_EDGE ( 'NONE', *, *, #11009, .T. ) ;
#18033 = CARTESIAN_POINT ( 'NONE',  ( -17.25000000000148503, -20.00000000000000000, -8.499999999996081357 ) ) ;
#18034 = FACE_OUTER_BOUND ( 'NONE', #9300, .T. ) ;
#18035 = DIRECTION ( 'NONE',  ( -0.9999862922474491711, -0.005235963827128305680, 1.187304881134278487E-16 ) ) ;
#18036 = ORIENTED_EDGE ( 'NONE', *, *, #10864, .F. ) ;
#18037 = EDGE_CURVE ( 'NONE', #17804, #22271, #23292, .T. ) ;
#18038 = CYLINDRICAL_SURFACE ( 'NONE', #11495, 2.066999999999998394 ) ;
#18039 = DIRECTION ( 'NONE',  ( -0.9730401042858035643, 0.2306359803922028717, 6.126766849694256332E-17 ) ) ;
#18040 = ORIENTED_EDGE ( 'NONE', *, *, #5273, .T. ) ;
#18041 = PERSON_AND_ORGANIZATION ( #11966, #8758 ) ;
#18042 = ORIENTED_EDGE ( 'NONE', *, *, #19847, .F. ) ;
#18043 = AXIS2_PLACEMENT_3D ( 'NONE', #13606, #22515, #10299 ) ;
#18044 = EDGE_LOOP ( 'NONE', ( #11697, #5350, #676, #5685 ) ) ;
#18045 = LINE ( 'NONE', #16253, #7313 ) ;
#18046 = PERSON_AND_ORGANIZATION_ROLE ( 'creator' ) ;
#18047 = ADVANCED_FACE ( 'NONE', ( #7122, #3198 ), #12120, .T. ) ;
#18048 = CARTESIAN_POINT ( 'NONE',  ( 52.26033179423370001, -7.535689554643980159, -13.00000000000039968 ) ) ;
#18049 = CALENDAR_DATE ( 2026, 31, 10 ) ;
#18050 = DIRECTION ( 'NONE',  ( 0.000000000000000000, -2.739767185169682068E-14, -1.000000000000000000 ) ) ;
#18051 = SHAPE_REPRESENTATION_RELATIONSHIP ( 'NONE' , 'NONE' ,  #7508, #1704 ) ;
#18052 = LINE ( 'NONE', #16379, #19467 ) ;
#18053 = APPLICATION_PROTOCOL_DEFINITION ( 'international standard', 'config_control_design', 1994, #5484 ) ;
#18054 = ORIENTED_EDGE ( 'NONE', *, *, #15496, .T. ) ;
#18055 = DIRECTION ( 'NONE',  ( 1.000000000000000000, -2.211842757264940144E-18, 0.000000000000000000 ) ) ;
#18056 = CARTESIAN_POINT ( 'NONE',  ( 115.1338136878955964, -20.09158224951067240, -13.00000000000000000 ) ) ;
#18057 = ORIENTED_EDGE ( 'NONE', *, *, #5555, .F. ) ;
#18058 = CIRCLE ( 'NONE', #21087, 2.066999999999998394 ) ;
#18059 = EDGE_CURVE ( 'NONE', #2209, #23363, #1398, .T. ) ;
#18060 = FACE_OUTER_BOUND ( 'NONE', #702, .T. ) ;
#18061 = FACE_OUTER_BOUND ( 'NONE', #21500, .T. ) ;
#18062 = LINE ( 'NONE', #19957, #11885 ) ;
#18063 = VERTEX_POINT ( 'NONE', #12360 ) ;
#18064 = ORIENTED_EDGE ( 'NONE', *, *, #21314, .F. ) ;
#18065 = CARTESIAN_POINT ( 'NONE',  ( -20.00000000000000000, -20.00000000000000000, -2.500000000000000000 ) ) ;
#18066 = ORIENTED_EDGE ( 'NONE', *, *, #18119, .F. ) ;
#18067 = APPROVAL ( #9461, 'UNKNOWN' ) ;
#18068 = COORDINATED_UNIVERSAL_TIME_OFFSET ( 0, 0, .AHEAD. ) ;
#18069 = ORIENTED_EDGE ( 'NONE', *, *, #1560, .F. ) ;
#18070 = ORIENTED_EDGE ( 'NONE', *, *, #23017, .F. ) ;
#18071 = CARTESIAN_POINT ( 'NONE',  ( 1.406882533891259834, 17.87809865158410005, -7.060250502199809043E-15 ) ) ;
#18072 = DIRECTION ( 'NONE',  ( 8.911056267098788616E-18, 1.998401444326210262E-15, 1.000000000000000000 ) ) ;
#18073 = DATE_AND_TIME ( #3590, #13736 ) ;
#18074 = EDGE_CURVE ( 'NONE', #2591, #16276, #6236, .T. ) ;
#18075 = LINE ( 'NONE', #9049, #5927 ) ;
#18076 = EDGE_CURVE ( 'NONE', #22844, #21777, #16066, .T. ) ;
#18077 = AXIS2_PLACEMENT_3D ( 'NONE', #11169, #18507, #14808 ) ;
#18078 = DIRECTION ( 'NONE',  ( -1.000000000000000000, -6.662112528310618598E-09, 2.269018306577664942E-13 ) ) ;
#18079 = AXIS2_PLACEMENT_3D ( 'NONE', #17333, #11657, #930 ) ;
#18080 = DIRECTION ( 'NONE',  ( 1.000000000000000000, 0.000000000000000000, 0.000000000000000000 ) ) ;
#18081 = ORIENTED_EDGE ( 'NONE', *, *, #19061, .T. ) ;
#18082 = FACE_OUTER_BOUND ( 'NONE', #18664, .T. ) ;
#18083 = APPROVAL_STATUS ( 'not_yet_approved' ) ;
#18084 = CARTESIAN_POINT ( 'NONE',  ( 34.07549947545459901, 22.01160333750090459, -14.50000000000050093 ) ) ;
#18085 = DIRECTION ( 'NONE',  ( 1.000000000000000000, 0.000000000000000000, 0.000000000000000000 ) ) ;
#18086 = CARTESIAN_POINT ( 'NONE',  ( -58.40940726287419693, -21.55617503030518023, -5.536226058455569256E-15 ) ) ;
#18087 = EDGE_CURVE ( 'NONE', #20341, #16220, #8502, .T. ) ;
#18088 = CIRCLE ( 'NONE', #8224, 2.500000000000000888 ) ;
#18089 = CARTESIAN_POINT ( 'NONE',  ( 0.000000000000000000, 1.250000000000000000, 5.000000000000000000 ) ) ;
#18090 = AXIS2_PLACEMENT_3D ( 'NONE', #22166, #10928, #190 ) ;
#18091 = CIRCLE ( 'NONE', #2544, 4.750000000000000000 ) ;
#18092 = CARTESIAN_POINT ( 'NONE',  ( -20.00000000000000000, -20.00000000000000000, -5.000000000000000000 ) ) ;
#18093 = ORIENTED_EDGE ( 'NONE', *, *, #5759, .T. ) ;
#18094 = CARTESIAN_POINT ( 'NONE',  ( -20.00000000000000000, -20.00000000000000000, 0.000000000000000000 ) ) ;
#18095 = PRODUCT_DEFINITION ( 'UNKNOWN', '', #8830, #18234 ) ;
#18096 = CC_DESIGN_PERSON_AND_ORGANIZATION_ASSIGNMENT ( #6411, #17453, ( #23156 ) ) ;
#18097 = ORIENTED_EDGE ( 'NONE', *, *, #13459, .F. ) ;
#18098 = CARTESIAN_POINT ( 'NONE',  ( -69.83648240813081998, -6.865755409778439677, 0.01852613985923039913 ) ) ;
#18099 = DIRECTION ( 'NONE',  ( 0.000000000000000000, 1.000000000000000000, 0.000000000000000000 ) ) ;
#18100 = ORIENTED_EDGE ( 'NONE', *, *, #158, .T. ) ;
#18101 = ADVANCED_FACE ( 'NONE', ( #12808 ), #7695, .T. ) ;
#18102 = CARTESIAN_POINT ( 'NONE',  ( -27.39127619791450030, 6.327883175579949615, -3.750000000000000000 ) ) ;
#18103 = ADVANCED_FACE ( 'NONE', ( #3892 ), #18156, .T. ) ;
#18104 = VERTEX_POINT ( 'NONE', #9476 ) ;
#18105 = CARTESIAN_POINT ( 'NONE',  ( 39.69419854219519550, 9.774809681453278998, 21.49999999999999289 ) ) ;
#18106 = AXIS2_PLACEMENT_3D ( 'NONE', #5038, #10512, #12064 ) ;
#18107 = APPROVAL_DATE_TIME ( #8860, #2538 ) ;
#18108 = CARTESIAN_POINT ( 'NONE',  ( 38.12041445833288122, 17.39768532946521162, -13.00000000000030020 ) ) ;
#18109 = AXIS2_PLACEMENT_3D ( 'NONE', #622, #5514, #21780 ) ;
#18110 = AXIS2_PLACEMENT_3D ( 'NONE', #20222, #21143, #6312 ) ;
#18111 = CARTESIAN_POINT ( 'NONE',  ( -4.514225866272970400, 4.676725866273559795, -2.500000000000000000 ) ) ;
#18112 = LINE ( 'NONE', #7310, #664 ) ;
#18113 = DATE_AND_TIME ( #3621, #9139 ) ;
#18114 = VECTOR ( 'NONE', #14764, 1000.000000000000114 ) ;
#18115 = CARTESIAN_POINT ( 'NONE',  ( 52.73786095581300515, -7.648876468381129889, 13.00000000000019895 ) ) ;
#18116 =( REPRESENTATION_RELATIONSHIP ('NONE','NONE', #18121, #12508 ) REPRESENTATION_RELATIONSHIP_WITH_TRANSFORMATION ( #17212 )SHAPE_REPRESENTATION_RELATIONSHIP( ) );
#18117 = CARTESIAN_POINT ( 'NONE',  ( 118.5310588935630136, -6.697506338400810222, 19.59999999999999787 ) ) ;
#18118 = DIRECTION ( 'NONE',  ( 0.2306359803922080898, 0.9730401042858024541, -2.572202231434325988E-16 ) ) ;
#18119 = EDGE_CURVE ( 'NONE', #18183, #20805, #10021, .T. ) ;
#18120 = CARTESIAN_POINT ( 'NONE',  ( -0.5391976746782148888, 18.33937061236850141, 3.301631463538509622E-17 ) ) ;
#18121 = SHAPE_REPRESENTATION ( 'Electric Motor', ( #10651, #4192, #376, #17069, #17461, #4959, #19363, #3, #13664, #3058 ), #8000 ) ;
#18122 = CIRCLE ( 'NONE', #13551, 2.500000000000000444 ) ;
#18123 = CARTESIAN_POINT ( 'NONE',  ( -20.00000000397270128, 22.95208919256889857, -4.999999999995559996 ) ) ;
#18124 = PLANE ( 'NONE',  #13744 ) ;
#18125 = ORIENTED_EDGE ( 'NONE', *, *, #18631, .T. ) ;
#18126 = AXIS2_PLACEMENT_3D ( 'NONE', #21324, #1361, #23213 ) ;
#18127 = EDGE_CURVE ( 'NONE', #645, #7554, #21818, .T. ) ;
#18128 = AXIS2_PLACEMENT_3D ( 'NONE', #17269, #22587, #8238 ) ;
#18129 = ORIENTED_EDGE ( 'NONE', *, *, #8760, .F. ) ;
#18130 = CARTESIAN_POINT ( 'NONE',  ( -20.00000000397129796, 22.95208919256900160, 6.500000000004299672 ) ) ;
#18131 = VECTOR ( 'NONE', #4818, 1000.000000000000227 ) ;
#18132 = DIRECTION ( 'NONE',  ( -0.9730401042858024541, 0.2306359803922080898, 5.959266323858942451E-17 ) ) ;
#18133 = ORIENTED_EDGE ( 'NONE', *, *, #20854, .T. ) ;
#18134 = ADVANCED_FACE ( 'NONE', ( #5552 ), #18038, .F. ) ;
#18135 = SECURITY_CLASSIFICATION_LEVEL ( 'unclassified' ) ;
#18136 = DIRECTION ( 'NONE',  ( -0.9730401042858036753, 0.2306359803922028995, 5.959266323858677443E-17 ) ) ;
#18137 = EDGE_LOOP ( 'NONE', ( #17417, #5378, #6485, #4512 ) ) ;
#18138 = ADVANCED_FACE ( 'NONE', ( #3764 ), #9013, .T. ) ;
#18139 = CARTESIAN_POINT ( 'NONE',  ( -30.72370968135370006, -6.660959539311599897, -2.999707106781269950 ) ) ;
#18140 = PERSON_AND_ORGANIZATION ( #11966, #8758 ) ;
#18141 = VECTOR ( 'NONE', #7335, 1000.000000000000114 ) ;
#18142 = CONTEXT_DEPENDENT_SHAPE_REPRESENTATION ( #10088, #6282 ) ;
#18143 = VECTOR ( 'NONE', #4033, 1000.000000000000000 ) ;
#18144 = CARTESIAN_POINT ( 'NONE',  ( 36.09092202081949807, 8.115512906978469942, 29.25000000000000000 ) ) ;
#18145 = FACE_BOUND ( 'NONE', #19479, .T. ) ;
#18146 = VERTEX_POINT ( 'NONE', #1748 ) ;
#18147 = PERSON ( 'NAUO-PER16', 'UNSPECIFIED', 'UNSPECIFIED', ('UNSPECIFIED'), ('UNSPECIFIED'), ('UNSPECIFIED') ) ;
#18148 = LINE ( 'NONE', #12691, #16625 ) ;
#18149 = ORIENTED_EDGE ( 'NONE', *, *, #10219, .F. ) ;
#18150 = CARTESIAN_POINT ( 'NONE',  ( 55.93909781928478253, -6.283383317918767474, 13.00000000000000000 ) ) ;
#18151 = CARTESIAN_POINT ( 'NONE',  ( 37.88245768368250310, -4.127756955731490152, 13.00000000000000000 ) ) ;
#18152 = CARTESIAN_POINT ( 'NONE',  ( -19.99975861755300244, 22.95209442650120124, 4.999999999999900524 ) ) ;
#18153 = ORIENTED_EDGE ( 'NONE', *, *, #4482, .T. ) ;
#18154 = APPROVAL ( #9411, 'UNSPECIFIED' ) ;
#18155 = DATE_TIME_ROLE ( 'classification_date' ) ;
#18156 = PLANE ( 'NONE',  #15638 ) ;
#18157 = VERTEX_POINT ( 'NONE', #11042 ) ;
#18158 = APPROVAL_STATUS ( 'not_yet_approved' ) ;
#18159 = ORIENTED_EDGE ( 'NONE', *, *, #6126, .T. ) ;
#18160 = ORIENTED_EDGE ( 'NONE', *, *, #13071, .T. ) ;
#18161 = DIRECTION ( 'NONE',  ( -8.623081276789554834E-17, -1.054188326053478339E-16, -1.000000000000000000 ) ) ;
#18162 = VECTOR ( 'NONE', #17051, 1000.000000000000114 ) ;
#18163 = PERSON_AND_ORGANIZATION ( #11966, #8758 ) ;
#18164 = ADVANCED_BREP_SHAPE_REPRESENTATION ( '', ( #9291, #12739 ), #210 ) ;
#18165 = PLANE ( 'NONE',  #20706 ) ;
#18166 = DIRECTION ( 'NONE',  ( 1.000000000000000000, 3.794988516547419626E-16, -1.751623080406019734E-47 ) ) ;
#18167 = EDGE_CURVE ( 'NONE', #306, #11069, #15828, .T. ) ;
#18168 = CYLINDRICAL_SURFACE ( 'NONE', #11129, 0.0009999999998218898900 ) ;
#18169 = CALENDAR_DATE ( 2026, 31, 10 ) ;
#18170 = ORIENTED_EDGE ( 'NONE', *, *, #1483, .T. ) ;
#18171 = LINE ( 'NONE', #10836, #21890 ) ;
#18172 = VERTEX_POINT ( 'NONE', #13054 ) ;
#18173 = DIRECTION ( 'NONE',  ( 0.1630842657209385649, 0.6880432561069587116, 0.7071067811865449082 ) ) ;
#18174 = DIRECTION ( 'NONE',  ( 3.099353312215988811E-62, 0.000000000000000000, -1.000000000000000000 ) ) ;
#18175 = CARTESIAN_POINT ( 'NONE',  ( -24.50000000000000000, -28.60000000000000142, -19.00000000000000000 ) ) ;
#18176 = EDGE_LOOP ( 'NONE', ( #8717, #14342, #9651, #601, #7837 ) ) ;
#18177 = SECURITY_CLASSIFICATION ( '', '', #98 ) ;
#18178 = ORIENTED_EDGE ( 'NONE', *, *, #919, .F. ) ;
#18180 = DIRECTION ( 'NONE',  ( 0.2306359803922080343, 0.9730401042858022320, -1.412237191019910313E-17 ) ) ;
#18179 = CIRCLE ( 'NONE', #20067, 2.386550000000003724 ) ;
#18181 = ORIENTED_EDGE ( 'NONE', *, *, #22321, .F. ) ;
#18182 = PERSON_AND_ORGANIZATION_ROLE ( 'design_supplier' ) ;
#18183 = VERTEX_POINT ( 'NONE', #195 ) ;
#18184 = ORIENTED_EDGE ( 'NONE', *, *, #16123, .T. ) ;
#18185 = CYLINDRICAL_SURFACE ( 'NONE', #20619, 2.500000000000000888 ) ;
#18186 = CARTESIAN_POINT ( 'NONE',  ( 45.07211867146970263, 28.08243186520990164, -13.00000000000000000 ) ) ;
#18187 = PERSON_AND_ORGANIZATION_ROLE ( 'design_owner' ) ;
#18188 = CARTESIAN_POINT ( 'NONE',  ( 114.8905747189829896, 12.63019305843990026, 2.920919059678259917E-14 ) ) ;
#18189 = LINE ( 'NONE', #12960, #7609 ) ;
#18190 = EDGE_CURVE ( 'NONE', #3674, #11869, #11175, .T. ) ;
#18191 = ORGANIZATION ( 'NAUO-ORG9', 'UNSPECIFIED', 'UNSPECIFIED' ) ;
#18192 = VECTOR ( 'NONE', #5831, 999.9999999999998863 ) ;
#18193 = ORIENTED_EDGE ( 'NONE', *, *, #8913, .T. ) ;
#18194 = DIRECTION ( 'NONE',  ( -4.028143194477080210E-16, -2.054129435991050111E-15, -1.000000000000000000 ) ) ;
#18195 = APPROVAL_STATUS ( 'not_yet_approved' ) ;
#18196 = ORIENTED_EDGE ( 'NONE', *, *, #12759, .F. ) ;
#18198 = DIRECTION ( 'NONE',  ( -1.000000000000000000, 0.000000000000000000, 0.000000000000000000 ) ) ;
#18197 = AXIS2_PLACEMENT_3D ( 'NONE', #14314, #12544, #22244 ) ;
#18199 = EDGE_CURVE ( 'NONE', #19582, #13450, #7723, .T. ) ;
#18200 = EDGE_CURVE ( 'NONE', #7455, #2399, #18751, .T. ) ;
#18201 = FACE_OUTER_BOUND ( 'NONE', #9815, .T. ) ;
#18202 = CARTESIAN_POINT ( 'NONE',  ( 39.76749112244890227, 5.702509466636359825, -15.90000000000000036 ) ) ;
#18203 = DIRECTION ( 'NONE',  ( 0.9730401042858036753, -0.2306359803922028995, -5.959266323858677443E-17 ) ) ;
#18204 = ORIENTED_EDGE ( 'NONE', *, *, #11334, .T. ) ;
#18205 = FACE_OUTER_BOUND ( 'NONE', #12612, .T. ) ;
#18206 = UNCERTAINTY_MEASURE_WITH_UNIT (LENGTH_MEASURE( 1.000000000000000082E-05 ), #16749, 'distance_accuracy_value', 'NONE');
#18207 = PRODUCT_DEFINITION_SHAPE ( 'NONE', 'NONE',  #15459 ) ;
#18208 = LOCAL_TIME ( 14, 11, 27.00000000000000000, #7715 ) ;
#18209 = EDGE_LOOP ( 'NONE', ( #20419, #3957 ) ) ;
#18210 = FACE_OUTER_BOUND ( 'NONE', #7835, .T. ) ;
#18211 = LINE ( 'NONE', #16423, #13262 ) ;
#18212 = VECTOR ( 'NONE', #17645, 1000.000000000000227 ) ;
#18213 = VERTEX_POINT ( 'NONE', #20400 ) ;
#18214 = CIRCLE ( 'NONE', #7980, 2.066999999999998394 ) ;
#18215 = DIRECTION ( 'NONE',  ( 2.269747459788994803E-13, 2.220446049250305192E-15, 1.000000000000000000 ) ) ;
#18216 = VERTEX_POINT ( 'NONE', #10812 ) ;
#18217 = DIRECTION ( 'NONE',  ( 4.040376328279780192E-15, -1.000000000000000000, 1.816625962794309743E-30 ) ) ;
#18218 = SECURITY_CLASSIFICATION_LEVEL ( 'unclassified' ) ;
#18219 = CARTESIAN_POINT ( 'NONE',  ( 35.59419854219520118, 9.774809681453358934, -10.99076000000050080 ) ) ;
#18220 = AXIS2_PLACEMENT_3D ( 'NONE', #16178, #3704, #18198 ) ;
#18221 = EDGE_CURVE ( 'NONE', #4745, #5829, #21003, .T. ) ;
#18222 = CIRCLE ( 'NONE', #1948, 2.499999999999998668 ) ;
#18223 = FACE_BOUND ( 'NONE', #4220, .T. ) ;
#18224 = APPROVAL ( #10295, 'UNSPECIFIED' ) ;
#18225 = CARTESIAN_POINT ( 'NONE',  ( 96.81657767996070163, -18.09668638014640152, -13.00000000000000000 ) ) ;
#18226 = CARTESIAN_POINT ( 'NONE',  ( 0.000000000000000000, 0.000000000000000000, 0.000000000000000000 ) ) ;
#18227 = LOCAL_TIME ( 14, 11, 27.00000000000000000, #18661 ) ;
#18228 = CC_DESIGN_PERSON_AND_ORGANIZATION_ASSIGNMENT ( #12344, #14567, ( #16369 ) ) ;
#18229 = CYLINDRICAL_SURFACE ( 'NONE', #3949, 5.000000000000000888 ) ;
#18230 = DIRECTION ( 'NONE',  ( 0.000000000000000000, 1.734723475976806848E-16, 1.000000000000000000 ) ) ;
#18231 = EDGE_CURVE ( 'NONE', #21488, #17995, #19115, .T. ) ;
#18232 = EDGE_CURVE ( 'NONE', #20891, #17891, #19932, .T. ) ;
#18233 = CARTESIAN_POINT ( 'NONE',  ( 43.66832999130209458, 21.22121844545429781, 13.00000000000000000 ) ) ;
#18234 = DESIGN_CONTEXT ( 'detailed design', #328, 'design' ) ;
#18235 = CYLINDRICAL_SURFACE ( 'NONE', #791, 8.000000000000003553 ) ;
#18236 = APPROVAL ( #17081, 'UNSPECIFIED' ) ;
#18238 = EDGE_CURVE ( 'NONE', #18259, #18172, #14813, .T. ) ;
#18237 = LINE ( 'NONE', #10658, #6198 ) ;
#18239 = DIRECTION ( 'NONE',  ( -0.2306359803922033713, -0.9730401042858034533, 4.558064749665356219E-15 ) ) ;
#18240 = AXIS2_PLACEMENT_3D ( 'NONE', #11743, #2689, #13617 ) ;
#18241 = ORIENTED_EDGE ( 'NONE', *, *, #9731, .F. ) ;
#18242 = VERTEX_POINT ( 'NONE', #22527 ) ;
#18243 = DIRECTION ( 'NONE',  ( -6.123237831918399306E-17, 2.152213273084510109E-30, 1.000000000000000000 ) ) ;
#18244 = DIRECTION ( 'NONE',  ( -0.9730401042858020100, 0.2306359803922089780, 0.000000000000000000 ) ) ;
#18245 = ORIENTED_EDGE ( 'NONE', *, *, #1729, .F. ) ;
#18246 = CARTESIAN_POINT ( 'NONE',  ( -1.262685242559879909E-14, -17.30000000000000071, 5.000000000000000000 ) ) ;
#18247 = ORIENTED_EDGE ( 'NONE', *, *, #18960, .F. ) ;
#18248 = CC_DESIGN_APPROVAL ( #7938, ( #16700 ) ) ;
#18249 = CARTESIAN_POINT ( 'NONE',  ( -17.47493719149670000, 26.45208920939580111, 8.000000000004430234 ) ) ;
#18250 = DIRECTION ( 'NONE',  ( -0.9999862922474493931, -0.005235963827116132258, 1.466966272681990539E-16 ) ) ;
#18251 = APPROVAL_STATUS ( 'not_yet_approved' ) ;
#18252 = CARTESIAN_POINT ( 'NONE',  ( 36.79306370352710331, 8.085618792784300624, -8.896078739569128757 ) ) ;
#18253 = EDGE_CURVE ( 'NONE', #1337, #187, #3557, .T. ) ;
#18254 = CC_DESIGN_SECURITY_CLASSIFICATION ( #17878, ( #23512 ) ) ;
#18255 = CALENDAR_DATE ( 2026, 31, 10 ) ;
#18256 = DIRECTION ( 'NONE',  ( -4.590283530086319968E-31, -4.798094407101261014E-15, -1.000000000000000000 ) ) ;
#18257 = ORIENTED_EDGE ( 'NONE', *, *, #14164, .F. ) ;
#18258 = AXIS2_PLACEMENT_3D ( 'NONE', #2073, #9324, #11248 ) ;
#18259 = VERTEX_POINT ( 'NONE', #779 ) ;
#18260 =( BOUNDED_CURVE ( )  B_SPLINE_CURVE ( 2, ( #15760, #2932, #6857 ),
 .UNSPECIFIED., .F., .F. ) 
 B_SPLINE_CURVE_WITH_KNOTS ( ( 3, 3 ),
 ( 0.000000000000000000, 0.2928548593876180162 ),
 .UNSPECIFIED. ) 
 CURVE ( )  GEOMETRIC_REPRESENTATION_ITEM ( )  RATIONAL_B_SPLINE_CURVE ( ( 1.000000000000000000, 1.037954849302019866, 1.000000000000000000 ) ) 
 REPRESENTATION_ITEM ( '' )  );
#18261 = CARTESIAN_POINT ( 'NONE',  ( -14.00000000000130029, -19.99999999944489915, -5.499999999996829203 ) ) ;
#18262 = VERTEX_POINT ( 'NONE', #4244 ) ;
#18263 = DIRECTION ( 'NONE',  ( 1.000000000000000000, 0.000000000000000000, 0.000000000000000000 ) ) ;
#18264 = ADVANCED_FACE ( 'NONE', ( #15397 ), #10081, .T. ) ;
#18265 = ADVANCED_FACE ( 'NONE', ( #6269 ), #9732, .T. ) ;
#18266 = APPROVAL_PERSON_ORGANIZATION ( #16705, #20272, #435 ) ;
#18267 = EDGE_LOOP ( 'NONE', ( #15988, #4495, #22767, #6688 ) ) ;
#18268 = CC_DESIGN_APPROVAL ( #6543, ( #3051 ) ) ;
#18269 = CYLINDRICAL_SURFACE ( 'NONE', #18077, 2.066999999999999726 ) ;
#18271 = AXIS2_PLACEMENT_3D ( 'NONE', #19126, #929, #6284 ) ;
#18270 = CARTESIAN_POINT ( 'NONE',  ( 38.35918225515318625, -2.116483060172758446, -13.00000000000000000 ) ) ;
#18272 = DIRECTION ( 'NONE',  ( 0.000000000000000000, 0.000000000000000000, -1.000000000000000000 ) ) ;
#18273 = ORIENTED_EDGE ( 'NONE', *, *, #15919, .F. ) ;
#18274 = DATE_AND_TIME ( #9610, #7308 ) ;
#18275 = CARTESIAN_POINT ( 'NONE',  ( 30.76933207471829590, -4.221800468112435922, 14.00000000000021672 ) ) ;
#18276 = LOCAL_TIME ( 14, 11, 27.00000000000000000, #762 ) ;
#18277 = ORIENTED_EDGE ( 'NONE', *, *, #4050, .T. ) ;
#18278 = DATE_AND_TIME ( #10934, #20525 ) ;
#18279 = ORIENTED_EDGE ( 'NONE', *, *, #15918, .F. ) ;
#18280 = ORIENTED_EDGE ( 'NONE', *, *, #21053, .F. ) ;
#18281 = DIRECTION ( 'NONE',  ( 0.000000000000000000, 1.000000000000000000, 0.000000000000000000 ) ) ;
#18282 = SECURITY_CLASSIFICATION_LEVEL ( 'unclassified' ) ;
#18283 = EDGE_CURVE ( 'NONE', #22247, #12473, #2345, .T. ) ;
#18284 = CC_DESIGN_SECURITY_CLASSIFICATION ( #5761, ( #3492 ) ) ;
#18285 = CARTESIAN_POINT ( 'NONE',  ( -19.49999999982360066, -0.1021026942259579962, 5.000000000000000000 ) ) ;
#18286 = DATE_AND_TIME ( #18049, #12141 ) ;
#18287 = DIRECTION ( 'NONE',  ( -0.9730401042858024541, 0.2306359803922080898, 5.959266323862662423E-17 ) ) ;
#18288 = AXIS2_PLACEMENT_3D ( 'NONE', #23305, #7063, #14286 ) ;
#18289 = ADVANCED_FACE ( 'NONE', ( #9840 ), #7931, .F. ) ;
#18290 = LOCAL_TIME ( 14, 11, 27.00000000000000000, #15502 ) ;
#18291 = CARTESIAN_POINT ( 'NONE',  ( 89.62416413250200264, 10.32848256004250054, -13.00000000000030020 ) ) ;
#18292 = EDGE_CURVE ( 'NONE', #12006, #8528, #8167, .T. ) ;
#18293 = DATE_AND_TIME ( #22184, #22360 ) ;
#18294 = AXIS2_PLACEMENT_3D ( 'NONE', #14265, #20075, #21503 ) ;
#18295 = ORIENTED_EDGE ( 'NONE', *, *, #19222, .T. ) ;
#18296 = DIRECTION ( 'NONE',  ( -0.1997366180463770735, -0.8426774492125654881, -0.4999999999999997780 ) ) ;
#18297 = ORIENTED_EDGE ( 'NONE', *, *, #13271, .F. ) ;
#18298 = CC_DESIGN_APPROVAL ( #16471, ( #5893 ) ) ;
#18299 = CARTESIAN_POINT ( 'NONE',  ( 33.27705887009690144, -3.036156860537199798, -13.00000000000039968 ) ) ;
#18300 = DIRECTION ( 'NONE',  ( -0.9730401042858022320, 0.2306359803922080343, 5.252801108490690349E-31 ) ) ;
#18301 = DIRECTION ( 'NONE',  ( -0.2306359803922028162, -0.9730401042858034533, 1.407521210652564497E-17 ) ) ;
#18302 = EDGE_LOOP ( 'NONE', ( #11103, #21360, #3302, #23212, #992, #10025, #12268, #17290 ) ) ;
#18303 = ORIENTED_EDGE ( 'NONE', *, *, #19845, .F. ) ;
#18304 = DIRECTION ( 'NONE',  ( 0.9730401042858036753, -0.2306359803922028995, -5.432877459303547669E-17 ) ) ;
#18305 = VECTOR ( 'NONE', #7626, 1000.000000000000114 ) ;
#18306 = VERTEX_POINT ( 'NONE', #2471 ) ;
#18307 = AXIS2_PLACEMENT_3D ( 'NONE', #16224, #2079, #10905 ) ;
#18308 = CALENDAR_DATE ( 2026, 31, 10 ) ;
#18309 = VERTEX_POINT ( 'NONE', #22401 ) ;
#18310 = ORIENTED_EDGE ( 'NONE', *, *, #2964, .F. ) ;
#18311 = DIRECTION ( 'NONE',  ( -2.270069654138870255E-15, -1.000000000000000000, -7.035747901516317327E-77 ) ) ;
#18312 = CARTESIAN_POINT ( 'NONE',  ( -19.99999999999849720, -20.00000000000000000, 6.500000000004389378 ) ) ;
#18313 = CALENDAR_DATE ( 2026, 31, 10 ) ;
#18314 = CARTESIAN_POINT ( 'NONE',  ( -23.49917714535047963, 22.87619892134707200, -5.000000000000060396 ) ) ;
#18315 = AXIS2_PLACEMENT_3D ( 'NONE', #23307, #3483, #12858 ) ;
#18316 = DIRECTION ( 'NONE',  ( -0.005235963827121952255, 0.9999862922474493931, -2.738476122049136279E-14 ) ) ;
#18317 = VECTOR ( 'NONE', #9020, 999.9999999999998863 ) ;
#18318 = VECTOR ( 'NONE', #21942, 1000.000000000000227 ) ;
#18319 = PRODUCT_RELATED_PRODUCT_CATEGORY ( 'detail', '', ( #10241 ) ) ;
#18320 = LOCAL_TIME ( 14, 11, 27.00000000000000000, #6472 ) ;
#18321 = AXIS2_PLACEMENT_3D ( 'NONE', #1292, #13998, #9864 ) ;
#18322 = AXIS2_PLACEMENT_3D ( 'NONE', #9903, #15349, #2169 ) ;
#18323 = EDGE_LOOP ( 'NONE', ( #19502, #21035, #22987, #13060 ) ) ;
#18324 = FACE_BOUND ( 'NONE', #5263, .T. ) ;
#18325 = CALENDAR_DATE ( 2026, 31, 10 ) ;
#18326 = VECTOR ( 'NONE', #15849, 1000.000000000000227 ) ;
#18327 = ORIENTED_EDGE ( 'NONE', *, *, #3485, .T. ) ;
#18328 = FACE_OUTER_BOUND ( 'NONE', #9044, .T. ) ;
#18329 = DIRECTION ( 'NONE',  ( -0.9730401042858024541, 0.2306359803922080898, 5.959266323858942451E-17 ) ) ;
#18330 = FACE_OUTER_BOUND ( 'NONE', #8345, .T. ) ;
#18331 = LINE ( 'NONE', #3950, #4058 ) ;
#18332 = CARTESIAN_POINT ( 'NONE',  ( 31.49419854219519976, 9.774809681453278998, 25.00000000000000000 ) ) ;
#18333 = ORIENTED_EDGE ( 'NONE', *, *, #13795, .F. ) ;
#18334 = CONICAL_SURFACE ( 'NONE', #11542, 2.283499999999998753, 0.7853981633974433940 ) ;
#18335 = CARTESIAN_POINT ( 'NONE',  ( 35.53134815212258246, 11.84531904168216343, 8.774963029737106623 ) ) ;
#18336 = VECTOR ( 'NONE', #15776, 1000.000000000000227 ) ;
#18337 = EDGE_CURVE ( 'NONE', #2620, #15994, #2696, .T. ) ;
#18338 = APPROVAL_PERSON_ORGANIZATION ( #3401, #347, #16231 ) ;
#18339 = VERTEX_POINT ( 'NONE', #22630 ) ;
#18340 = ORIENTED_EDGE ( 'NONE', *, *, #10616, .F. ) ;
#18341 = CARTESIAN_POINT ( 'NONE',  ( -16.00004797695752501, -0.08377682083102050425, -2.500000000000000444 ) ) ;
#18342 = CARTESIAN_POINT ( 'NONE',  ( 45.41807264205800010, 29.54199202163849947, -9.133960000000000079 ) ) ;
#18343 = ORIENTED_EDGE ( 'NONE', *, *, #20132, .T. ) ;
#18344 = AXIS2_PLACEMENT_3D ( 'NONE', #19263, #8334, #11486 ) ;
#18345 = AXIS2_PLACEMENT_3D ( 'NONE', #23289, #7047, #19732 ) ;
#18346 = DIRECTION ( 'NONE',  ( 2.199957270157979832E-13, -9.825194207785550278E-30, -1.000000000000000000 ) ) ;
#18347 = VERTEX_POINT ( 'NONE', #6143 ) ;
#18348 = VECTOR ( 'NONE', #10991, 1000.000000000000227 ) ;
#18349 = CARTESIAN_POINT ( 'NONE',  ( 6.500000000000000000, 0.000000000000000000, -2.500000000000000000 ) ) ;
#18350 = COORDINATED_UNIVERSAL_TIME_OFFSET ( 0, 0, .AHEAD. ) ;
#18351 = DIRECTION ( 'NONE',  ( 6.123230174520380038E-17, 4.962644601432250805E-15, 1.000000000000000000 ) ) ;
#18352 = EDGE_CURVE ( 'NONE', #16389, #14157, #511, .T. ) ;
#18353 = EDGE_CURVE ( 'NONE', #5108, #10034, #14296, .T. ) ;
#18354 = AXIS2_PLACEMENT_3D ( 'NONE', #16165, #23396, #9159 ) ;
#18355 = DIRECTION ( 'NONE',  ( -0.2306359803922028995, -0.9730401042858035643, -1.064172857958375654E-32 ) ) ;
#18356 = CARTESIAN_POINT ( 'NONE',  ( 37.46113131852679601, -4.027891576221570347, 20.00000000000000000 ) ) ;
#18357 = CALENDAR_DATE ( 2026, 31, 10 ) ;
#18358 = CIRCLE ( 'NONE', #8120, 0.4000000000000010214 ) ;
#18359 = FACE_OUTER_BOUND ( 'NONE', #20515, .T. ) ;
#18360 = AXIS2_PLACEMENT_3D ( 'NONE', #11660, #20658, #6524 ) ;
#18361 = DIRECTION ( 'NONE',  ( -0.9730401042858035643, 0.2306359803922028717, 5.958148513035547083E-17 ) ) ;
#18362 = FACE_OUTER_BOUND ( 'NONE', #15341, .T. ) ;
#18363 = FACE_OUTER_BOUND ( 'NONE', #3827, .T. ) ;
#18364 = DIRECTION ( 'NONE',  ( 1.138590270679730064E-14, 2.220446049251235259E-15, 1.000000000000000000 ) ) ;
#18365 = CARTESIAN_POINT ( 'NONE',  ( 38.67394081127452665, 19.73298157975111877, -13.00000000000049916 ) ) ;
#18366 = EDGE_LOOP ( 'NONE', ( #22809, #14433, #21706, #4345, #17318, #1862, #433, #8700 ) ) ;
#18367 = ADVANCED_FACE ( 'NONE', ( #11638 ), #1643, .F. ) ;
#18368 = ORIENTED_EDGE ( 'NONE', *, *, #4750, .F. ) ;
#18369 = FACE_BOUND ( 'NONE', #2939, .T. ) ;
#18370 = CARTESIAN_POINT ( 'NONE',  ( 39.83668191656649782, 5.994421497922140851, 18.89999999999999858 ) ) ;
#18371 = VERTEX_POINT ( 'NONE', #20510 ) ;
#18372 = PRODUCT_RELATED_PRODUCT_CATEGORY ( 'detail', '', ( #17082 ) ) ;
#18373 = LINE ( 'NONE', #5644, #3518 ) ;
#18374 = CIRCLE ( 'NONE', #20638, 6.500000000000000000 ) ;
#18375 = ORIENTED_EDGE ( 'NONE', *, *, #11122, .F. ) ;
#18376 = APPROVAL ( #13818, 'UNSPECIFIED' ) ;
#18377 = FACE_BOUND ( 'NONE', #700, .T. ) ;
#18378 = PERSON_AND_ORGANIZATION_ROLE ( 'design_owner' ) ;
#18379 = DIRECTION ( 'NONE',  ( 0.000000000000000000, 0.000000000000000000, -1.000000000000000000 ) ) ;
#18380 = EDGE_CURVE ( 'NONE', #2609, #15201, #22752, .T. ) ;
#18381 = EDGE_CURVE ( 'NONE', #12811, #12690, #559, .T. ) ;
#18382 = APPROVAL_ROLE ( '' ) ;
#18383 =( NAMED_UNIT ( * ) SI_UNIT ( $, .STERADIAN. ) SOLID_ANGLE_UNIT ( ) );
#18384 = ORIENTED_EDGE ( 'NONE', *, *, #17625, .T. ) ;
#18385 = CARTESIAN_POINT ( 'NONE',  ( 35.59419854219520118, 9.774809681453278998, 23.00000000000000000 ) ) ;
#18386 = ORIENTED_EDGE ( 'NONE', *, *, #7670, .T. ) ;
#18387 = DIRECTION ( 'NONE',  ( 0.2867834340965190743, -0.9579954394086682701, 4.640009386119481531E-15 ) ) ;
#18388 = ORIENTED_EDGE ( 'NONE', *, *, #16937, .T. ) ;
#18389 = CARTESIAN_POINT ( 'NONE',  ( 33.37436288052550282, -3.059220458576433099, -15.50000000000040146 ) ) ;
#18390 = CARTESIAN_POINT ( 'NONE',  ( 35.13079550495196912, 7.819738582318153775, -10.50000000000049027 ) ) ;
#18391 = CARTESIAN_POINT ( 'NONE',  ( 35.09206298776550170, 20.88063091279809669, -13.00000000000049916 ) ) ;
#18392 = ORIENTED_EDGE ( 'NONE', *, *, #2852, .T. ) ;
#18393 = APPLICATION_CONTEXT ( 'configuration controlled 3d designs of mechanical parts and assemblies' ) ;
#18394 = EDGE_CURVE ( 'NONE', #8752, #4805, #8876, .T. ) ;
#18395 = CONTEXT_DEPENDENT_SHAPE_REPRESENTATION ( #13708, #9714 ) ;
#18396 = CARTESIAN_POINT ( 'NONE',  ( -24.50000000000000000, -30.47499999999999787, -19.00000000000000000 ) ) ;
#18397 = ORIENTED_EDGE ( 'NONE', *, *, #17504, .T. ) ;
#18399 = APPROVAL_STATUS ( 'not_yet_approved' ) ;
#18398 = CC_DESIGN_PERSON_AND_ORGANIZATION_ASSIGNMENT ( #21825, #17931, ( #13107 ) ) ;
#18400 = DIRECTION ( 'NONE',  ( 0.000000000000000000, 0.000000000000000000, 1.000000000000000000 ) ) ;
#18401 = EDGE_LOOP ( 'NONE', ( #6382, #20312 ) ) ;
#18402 = EDGE_LOOP ( 'NONE', ( #19667, #15323, #16757, #19410 ) ) ;
#18403 = CC_DESIGN_PERSON_AND_ORGANIZATION_ASSIGNMENT ( #20546, #7730, ( #22008 ) ) ;
#18404 = CARTESIAN_POINT ( 'NONE',  ( -19.49999999982360066, -0.1021026942259809916, -5.000000000000000000 ) ) ;
#18405 = DATE_AND_TIME ( #21480, #4649 ) ;
#18406 = EDGE_CURVE ( 'NONE', #18419, #1137, #2795, .T. ) ;
#18407 = EDGE_CURVE ( 'NONE', #4802, #7660, #16836, .T. ) ;
#18408 = CIRCLE ( 'NONE', #2077, 2.499999999999998668 ) ;
#18409 = FACE_OUTER_BOUND ( 'NONE', #20775, .T. ) ;
#18410 = DATE_AND_TIME ( #2008, #17813 ) ;
#18411 =( BOUNDED_CURVE ( )  B_SPLINE_CURVE ( 2, ( #19132, #16973, #2848 ),
 .UNSPECIFIED., .F., .F. ) 
 B_SPLINE_CURVE_WITH_KNOTS ( ( 3, 3 ),
 ( 0.000000000000000000, 0.5842180690389588982 ),
 .UNSPECIFIED. ) 
 CURVE ( )  GEOMETRIC_REPRESENTATION_ITEM ( )  RATIONAL_B_SPLINE_CURVE ( ( 1.000000000000000000, 1.154700538379249908, 1.000000000000000000 ) ) 
 REPRESENTATION_ITEM ( '' )  );
#18412 = CARTESIAN_POINT ( 'NONE',  ( 33.54350891239443655, 19.76716536178343731, -13.00000000000049916 ) ) ;
#18413 =( NAMED_UNIT ( * ) PLANE_ANGLE_UNIT ( ) SI_UNIT ( $, .RADIAN. ) );
#18414 = DIRECTION ( 'NONE',  ( -0.9999863470142589250, -0.005225493764064552404, 0.000000000000000000 ) ) ;
#18415 = DATE_TIME_ROLE ( 'creation_date' ) ;
#18416 = PRODUCT ( '1602p_c_10', '1602p_c_10', '', ( #16956 ) ) ;
#18417 = VERTEX_POINT ( 'NONE', #22283 ) ;
#18418 = DIRECTION ( 'NONE',  ( 0.9999862922474493931, 0.005235963827108152530, 0.000000000000000000 ) ) ;
#18419 = VERTEX_POINT ( 'NONE', #23225 ) ;
#18420 = PERSON ( 'NAUO-PER21', 'UNSPECIFIED', 'UNSPECIFIED', ('UNSPECIFIED'), ('UNSPECIFIED'), ('UNSPECIFIED') ) ;
#18421 = ADVANCED_FACE ( 'NONE', ( #10550 ), #13976, .T. ) ;
#18422 = CARTESIAN_POINT ( 'NONE',  ( 113.2033677465029911, -29.17473274740279976, -13.00000000000000000 ) ) ;
#18423 = AXIS2_PLACEMENT_3D ( 'NONE', #3156, #20968, #17296 ) ;
#18424 = DIRECTION ( 'NONE',  ( -0.9730401042858022320, 0.2306359803922080343, 5.959266323858941219E-17 ) ) ;
#18425 = FACE_OUTER_BOUND ( 'NONE', #3364, .T. ) ;
#18426 = ORIENTED_EDGE ( 'NONE', *, *, #11716, .F. ) ;
#18427 = ORIENTED_EDGE ( 'NONE', *, *, #2122, .T. ) ;
#18428 = DIRECTION ( 'NONE',  ( 0.9730401042858035643, -0.2306359803922028717, -5.432877459303547053E-17 ) ) ;
#18429 = ORIENTED_EDGE ( 'NONE', *, *, #11567, .F. ) ;
#18430 = APPLICATION_PROTOCOL_DEFINITION ( 'international standard', 'config_control_design', 1994, #2331 ) ;
#18431 = ADVANCED_FACE ( 'NONE', ( #15985, #22879 ), #6990, .T. ) ;
#18432 = ORIENTED_EDGE ( 'NONE', *, *, #3883, .T. ) ;
#18433 = VERTEX_POINT ( 'NONE', #8403 ) ;
#18434 = CARTESIAN_POINT ( 'NONE',  ( 36.10037903421270755, -9.768828191507928693, 2.700000000000049916 ) ) ;
#18435 = FACE_OUTER_BOUND ( 'NONE', #12346, .T. ) ;
#18436 = PERSON_AND_ORGANIZATION_ROLE ( 'creator' ) ;
#18437 = EDGE_CURVE ( 'NONE', #17265, #20139, #14213, .T. ) ;
#18438 = CARTESIAN_POINT ( 'NONE',  ( 66.60056952104010008, 2.425487965306460048, 1.173314102775059961E-14 ) ) ;
#18439 = EDGE_CURVE ( 'NONE', #14586, #7803, #10317, .T. ) ;
#18440 = DIRECTION ( 'NONE',  ( 1.000000000000000000, 9.794583108699330061E-17, 0.000000000000000000 ) ) ;
#18441 =( LENGTH_UNIT ( ) NAMED_UNIT ( * ) SI_UNIT ( .MILLI., .METRE. ) );
#18442 = ORIENTED_EDGE ( 'NONE', *, *, #6640, .T. ) ;
#18443 = AXIS2_PLACEMENT_3D ( 'NONE', #203, #3906, #10940 ) ;
#18444 = CYLINDRICAL_SURFACE ( 'NONE', #682, 4.250000000000001776 ) ;
#18445 = DATE_AND_TIME ( #16517, #4991 ) ;
#18446 = ORIENTED_EDGE ( 'NONE', *, *, #15808, .F. ) ;
#18447 = CARTESIAN_POINT ( 'NONE',  ( 36.09092202081949807, 8.115512906978191054, -27.69000000000049866 ) ) ;
#18448 = DIRECTION ( 'NONE',  ( -2.269747459788994803E-13, -2.220446049250320181E-15, -1.000000000000000000 ) ) ;
#18449 = FACE_BOUND ( 'NONE', #20060, .T. ) ;
#18450 = CARTESIAN_POINT ( 'NONE',  ( 106.2939232160746883, -18.21879530321555052, -13.00000000000000000 ) ) ;
#18451 = CARTESIAN_POINT ( 'NONE',  ( -20.00000000397270128, 22.95208919257349933, 6.750000000004470202 ) ) ;
#18452 = ORIENTED_EDGE ( 'NONE', *, *, #5222, .T. ) ;
#18453 = DIRECTION ( 'NONE',  ( -0.9730401042858035643, 0.2306359803922028717, 6.126766849694256332E-17 ) ) ;
#18454 = DESIGN_CONTEXT ( 'detailed design', #2914, 'design' ) ;
#18455 = CC_DESIGN_PERSON_AND_ORGANIZATION_ASSIGNMENT ( #4881, #19147, ( #10832 ) ) ;
#18456 = AXIS2_PLACEMENT_3D ( 'NONE', #22041, #11275, #78 ) ;
#18457 = EDGE_LOOP ( 'NONE', ( #22577, #20200, #16526, #14529 ) ) ;
#18458 = ORIENTED_EDGE ( 'NONE', *, *, #11916, .T. ) ;
#18459 = CARTESIAN_POINT ( 'NONE',  ( -20.00000000397360012, 22.95208919256889857, -3.750000000000000000 ) ) ;
#18460 = DIRECTION ( 'NONE',  ( -8.623081276789554834E-17, -1.054188326053478339E-16, -1.000000000000000000 ) ) ;
#18461 = ORIENTED_EDGE ( 'NONE', *, *, #13196, .F. ) ;
#18462 = DIRECTION ( 'NONE',  ( -5.964507377817269296E-17, -4.861311874385510251E-15, -1.000000000000000000 ) ) ;
#18463 = FACE_OUTER_BOUND ( 'NONE', #5802, .T. ) ;
#18464 = CALENDAR_DATE ( 2026, 31, 10 ) ;
#18465 = DIRECTION ( 'NONE',  ( 0.9999862922474492821, 0.005235963827121822151, -1.466966272681990292E-16 ) ) ;
#18466 = CARTESIAN_POINT ( 'NONE',  ( -19.19277407259999180, 26.35772955756921121, -5.465517275973897116E-15 ) ) ;
#18467 = EDGE_CURVE ( 'NONE', #19614, #11427, #14090, .T. ) ;
#18468 = FACE_BOUND ( 'NONE', #11519, .T. ) ;
#18469 = APPROVAL_STATUS ( 'not_yet_approved' ) ;
#18470 = VECTOR ( 'NONE', #20857, 999.9999999999998863 ) ;
#18471 = AXIS2_PLACEMENT_3D ( 'NONE', #1451, #12301, #2787 ) ;
#18472 = AXIS2_PLACEMENT_3D ( 'NONE', #20567, #13216, #20448 ) ;
#18473 = CARTESIAN_POINT ( 'NONE',  ( -20.00000000000000000, -20.00000000000000000, -5.000000000000000000 ) ) ;
#18474 = CARTESIAN_POINT ( 'NONE',  ( 120.6036919168680015, 2.985523383783569962, 13.00000000000000000 ) ) ;
#18475 = CARTESIAN_POINT ( 'NONE',  ( -68.69007546624879978, 8.433449002107520798, 2.873144230283079984E-15 ) ) ;
#18476 = CARTESIAN_POINT ( 'NONE',  ( 37.27955344062029752, 9.375336445360778370, 27.68999999999999773 ) ) ;
#18477 = DIRECTION ( 'NONE',  ( 1.187319687680494078E-16, 2.805478249478345354E-20, 1.000000000000000000 ) ) ;
#18478 = CARTESIAN_POINT ( 'NONE',  ( 29.36184298829660122, -3.294841866349869974, -11.00000000000039968 ) ) ;
#18479 = ORIENTED_EDGE ( 'NONE', *, *, #3485, .F. ) ;
#18480 = ORIENTED_EDGE ( 'NONE', *, *, #7826, .T. ) ;
#18481 = DIRECTION ( 'NONE',  ( 0.2306359803922030938, 0.9730401042858035643, -4.741332172907964454E-18 ) ) ;
#18482 = CARTESIAN_POINT ( 'NONE',  ( 35.27327876533596651, 27.06496614392695932, -13.00000000000049916 ) ) ;
#18483 = AXIS2_PLACEMENT_3D ( 'NONE', #11455, #8114, #6076 ) ;
#18484 = ORIENTED_EDGE ( 'NONE', *, *, #13032, .F. ) ;
#18485 = CARTESIAN_POINT ( 'NONE',  ( 32.12387896813558541, -7.901357381965519622, 13.00000000000000000 ) ) ;
#18486 = ORIENTED_EDGE ( 'NONE', *, *, #18283, .F. ) ;
#18487 = DIRECTION ( 'NONE',  ( -1.466984912809907930E-16, -2.805478249466190329E-20, -1.000000000000000000 ) ) ;
#18488 = CIRCLE ( 'NONE', #1016, 3.750000000000000000 ) ;
#18489 = CALENDAR_DATE ( 2026, 31, 10 ) ;
#18490 = CARTESIAN_POINT ( 'NONE',  ( 36.57968191736579655, 11.59683649233991964, -8.774963029737127940 ) ) ;
#18491 = APPROVAL_ROLE ( '' ) ;
#18492 = VECTOR ( 'NONE', #20241, 1000.000000000000000 ) ;
#18493 = CALENDAR_DATE ( 2026, 31, 10 ) ;
#18494 = CARTESIAN_POINT ( 'NONE',  ( -27.00000000000000000, -20.00000000000000000, 2.500000000000000000 ) ) ;
#18495 = VERTEX_POINT ( 'NONE', #21451 ) ;
#18496 = EDGE_CURVE ( 'NONE', #13515, #20139, #1371, .T. ) ;
#18497 = CIRCLE ( 'NONE', #17754, 5.000000000000001776 ) ;
#18498 = LINE ( 'NONE', #2211, #5085 ) ;
#18499 = ORIENTED_EDGE ( 'NONE', *, *, #4901, .F. ) ;
#18500 = LINE ( 'NONE', #13264, #15116 ) ;
#18501 = CC_DESIGN_DATE_AND_TIME_ASSIGNMENT ( #18613, #894, ( #12599 ) ) ;
#18502 = CIRCLE ( 'NONE', #2946, 2.500000000000000444 ) ;
#18503 = AXIS2_PLACEMENT_3D ( 'NONE', #3966, #16540, #265 ) ;
#18504 = DIRECTION ( 'NONE',  ( -5.742930707022404410E-47, 9.378911720669089789E-31, 1.000000000000000000 ) ) ;
#18505 = CIRCLE ( 'NONE', #17367, 6.000000000000109246 ) ;
#18506 = ORIENTED_EDGE ( 'NONE', *, *, #5261, .T. ) ;
#18507 = DIRECTION ( 'NONE',  ( 0.2306359803922080898, 0.9730401042858024541, -2.572202231434325988E-16 ) ) ;
#18508 = CYLINDRICAL_SURFACE ( 'NONE', #9176, 49.22658835543909817 ) ;
#18509 = DIRECTION ( 'NONE',  ( -0.2306359803922032603, -0.9730401042858034533, 0.000000000000000000 ) ) ;
#18510 = ORIENTED_EDGE ( 'NONE', *, *, #351, .F. ) ;
#18511 = ADVANCED_FACE ( 'NONE', ( #12438 ), #21208, .F. ) ;
#18512 = EDGE_CURVE ( 'NONE', #8379, #7119, #17601, .T. ) ;
#18513 = CALENDAR_DATE ( 2026, 31, 10 ) ;
#18514 = DIRECTION ( 'NONE',  ( 1.000000000000000000, -5.944927207247209745E-47, -9.694713396002079468E-78 ) ) ;
#18515 = AXIS2_PLACEMENT_3D ( 'NONE', #14676, #20267, #3868 ) ;
#18516 = ORIENTED_EDGE ( 'NONE', *, *, #783, .F. ) ;
#18517 = PERSON_AND_ORGANIZATION ( #11966, #8758 ) ;
#18518 = DIRECTION ( 'NONE',  ( 0.9999862922474491711, 0.005235963827117207786, -1.514467536079854800E-31 ) ) ;
#18519 = ORIENTED_EDGE ( 'NONE', *, *, #22296, .T. ) ;
#18520 = ORIENTED_EDGE ( 'NONE', *, *, #14075, .T. ) ;
#18521 = CARTESIAN_POINT ( 'NONE',  ( 29.35071467092108577, -7.244044837847879670, -13.00000000000000000 ) ) ;
#18522 = AXIS2_PLACEMENT_3D ( 'NONE', #2570, #15143, #16932 ) ;
#18523 = DATE_AND_TIME ( #22293, #15255 ) ;
#18524 = VECTOR ( 'NONE', #14896, 999.9999999999998863 ) ;
#18525 = CIRCLE ( 'NONE', #8281, 7.999999999999998224 ) ;
#18526 = DIRECTION ( 'NONE',  ( -0.2306359803922028995, -0.9730401042858036753, 1.343075398093749487E-16 ) ) ;
#18527 = ADVANCED_FACE ( 'NONE', ( #6630 ), #1136, .F. ) ;
#18528 = DIRECTION ( 'NONE',  ( 0.000000000000000000, 0.000000000000000000, -1.000000000000000000 ) ) ;
#18529 = PRODUCT_RELATED_PRODUCT_CATEGORY ( 'detail', '', ( #11806 ) ) ;
#18530 = DATE_AND_TIME ( #16490, #741 ) ;
#18531 = PRODUCT_DEFINITION ( 'UNKNOWN', '', #14088, #19902 ) ;
#18532 = ORIENTED_EDGE ( 'NONE', *, *, #5726, .T. ) ;
#18533 = CYLINDRICAL_SURFACE ( 'NONE', #23178, 6.000000000000000000 ) ;
#18534 = ORIENTED_EDGE ( 'NONE', *, *, #17194, .T. ) ;
#18535 = ADVANCED_FACE ( 'NONE', ( #17669 ), #19206, .F. ) ;
#18536 = EDGE_CURVE ( 'NONE', #8168, #22271, #18260, .T. ) ;
#18537 = LINE ( 'NONE', #15074, #1791 ) ;
#18538 = CC_DESIGN_DATE_AND_TIME_ASSIGNMENT ( #23059, #18571, ( #20495 ) ) ;
#18540 = VECTOR ( 'NONE', #3240, 999.9999999999998863 ) ;
#18539 = DIRECTION ( 'NONE',  ( -0.005235963827121941846, 0.9999862922474492821, 0.000000000000000000 ) ) ;
#18541 = DIRECTION ( 'NONE',  ( 3.330999558972852107E-36, 2.805478249484880275E-20, 1.000000000000000000 ) ) ;
#18542 = VERTEX_POINT ( 'NONE', #13862 ) ;
#18543 = EDGE_LOOP ( 'NONE', ( #3762, #20716, #10311, #9031 ) ) ;
#18544 = CARTESIAN_POINT ( 'NONE',  ( 36.88454136754629786, -6.460491836936129495, -2.999999999999930278 ) ) ;
#18545 = ORIENTED_EDGE ( 'NONE', *, *, #7899, .F. ) ;
#18546 = PERSON_AND_ORGANIZATION ( #11966, #8758 ) ;
#18547 = EDGE_LOOP ( 'NONE', ( #18030, #9330, #12937, #14379 ) ) ;
#18548 = VERTEX_POINT ( 'NONE', #12339 ) ;
#18549 = DIRECTION ( 'NONE',  ( 3.210834492181040124E-17, -2.441916418604790135E-15, -1.000000000000000000 ) ) ;
#18550 =( BOUNDED_CURVE ( )  B_SPLINE_CURVE ( 2, ( #2686, #419, #7681 ),
 .UNSPECIFIED., .F., .F. ) 
 B_SPLINE_CURVE_WITH_KNOTS ( ( 3, 3 ),
 ( 0.000000000000000000, 0.1168436138077928454 ),
 .UNSPECIFIED. ) 
 CURVE ( )  GEOMETRIC_REPRESENTATION_ITEM ( )  RATIONAL_B_SPLINE_CURVE ( ( 1.000000000000000000, 1.077350269189624843, 1.077350269189624843 ) ) 
 REPRESENTATION_ITEM ( '' )  );
#18551 = CARTESIAN_POINT ( 'NONE',  ( -20.00000000397420052, 22.95208919256889857, -6.499999999995379696 ) ) ;
#18552 = COORDINATED_UNIVERSAL_TIME_OFFSET ( 0, 0, .AHEAD. ) ;
#18553 = CARTESIAN_POINT ( 'NONE',  ( 3.499952022866072543, 0.01832587339492648335, -8.931114213653268455E-14 ) ) ;
#18554 = DIRECTION ( 'NONE',  ( 5.964507377817298878E-17, 4.861311874385510251E-15, 1.000000000000000000 ) ) ;
#18555 = ADVANCED_FACE ( 'NONE', ( #6745 ), #21336, .T. ) ;
#18556 = CLOSED_SHELL ( 'NONE', ( #18367, #19694, #7389, #19684, #12828, #15360, #14973, #10090, #18708, #22489, #22614, #10755, #5865, #6728, #7222, #6742, #17827, #10561, #12517, #18511, #3619 ) ) ;
#18557 = EDGE_LOOP ( 'NONE', ( #12362, #2617, #2934, #5929 ) ) ;
#18558 = DIRECTION ( 'NONE',  ( -8.911056267098788616E-18, -1.998401444326210262E-15, -1.000000000000000000 ) ) ;
#18559 = PERSON_AND_ORGANIZATION_ROLE ( 'classification_officer' ) ;
#18560 = ADVANCED_FACE ( 'NONE', ( #19558 ), #17777, .F. ) ;
#18561 = ORIENTED_EDGE ( 'NONE', *, *, #3358, .F. ) ;
#18562 = LINE ( 'NONE', #20794, #20874 ) ;
#18563 = AXIS2_PLACEMENT_3D ( 'NONE', #14061, #13839, #16083 ) ;
#18564 = PLANE ( 'NONE',  #21113 ) ;
#18565 = EDGE_CURVE ( 'NONE', #17206, #17836, #10201, .T. ) ;
#18566 = LINE ( 'NONE', #494, #21495 ) ;
#18567 = ADVANCED_FACE ( 'NONE', ( #20986 ), #20019, .F. ) ;
#18568 = CARTESIAN_POINT ( 'NONE',  ( -20.00000000397270128, 22.95208919257159863, 5.000000000004460432 ) ) ;
#18569 = VERTEX_POINT ( 'NONE', #5529 ) ;
#18570 = FACE_OUTER_BOUND ( 'NONE', #19120, .T. ) ;
#18571 = DATE_TIME_ROLE ( 'classification_date' ) ;
#18572 = ORIENTED_EDGE ( 'NONE', *, *, #14638, .F. ) ;
#18573 = ORIENTED_EDGE ( 'NONE', *, *, #12997, .T. ) ;
#18574 = FACE_OUTER_BOUND ( 'NONE', #12236, .T. ) ;
#18575 = DIRECTION ( 'NONE',  ( 2.982858504577240114E-17, -2.441916418604790135E-15, -1.000000000000000000 ) ) ;
#18576 =( REPRESENTATION_RELATIONSHIP ('NONE','NONE', #23243, #11914 ) REPRESENTATION_RELATIONSHIP_WITH_TRANSFORMATION ( #17789 )SHAPE_REPRESENTATION_RELATIONSHIP( ) );
#18577 = ORIENTED_EDGE ( 'NONE', *, *, #22028, .T. ) ;
#18578 = MECHANICAL_CONTEXT ( 'NONE', #11890, 'mechanical' ) ;
#18579 = CARTESIAN_POINT ( 'NONE',  ( 37.91003399039540511, 9.225896048120105775, 29.25000000000000355 ) ) ;
#18580 = CARTESIAN_POINT ( 'NONE',  ( 0.000000000000000000, 2.220446049250309925E-15, -5.000000000000000000 ) ) ;
#18581 = CC_DESIGN_APPROVAL ( #14153, ( #6423 ) ) ;
#18582 = CALENDAR_DATE ( 2026, 31, 10 ) ;
#18583 = AXIS2_PLACEMENT_3D ( 'NONE', #3609, #10878, #13568 ) ;
#18584 = CARTESIAN_POINT ( 'NONE',  ( 52.45828777336790694, 19.13776831658130106, 13.00000000000000000 ) ) ;
#18585 =( NAMED_UNIT ( * ) PLANE_ANGLE_UNIT ( ) SI_UNIT ( $, .RADIAN. ) );
#18586 = DIRECTION ( 'NONE',  ( -0.2306359803922009288, -0.9730401042858040084, 0.000000000000000000 ) ) ;
#18587 = CARTESIAN_POINT ( 'NONE',  ( -28.52462712253550237, 6.350733138482030249, 0.7325259402521719920 ) ) ;
#18588 = APPROVAL_ROLE ( '' ) ;
#18589 = CARTESIAN_POINT ( 'NONE',  ( 36.84099409957980242, 22.83947580187480142, 17.25000000000000000 ) ) ;
#18590 = DIRECTION ( 'NONE',  ( 0.2306359803922031215, 0.9730401042858033422, -4.741332172907962143E-18 ) ) ;
#18591 = EDGE_CURVE ( 'NONE', #9721, #7012, #11254, .T. ) ;
#18592 = CARTESIAN_POINT ( 'NONE',  ( -19.19277407259999180, 26.35772955756921121, 2.500000000000000000 ) ) ;
#18593 = CARTESIAN_POINT ( 'NONE',  ( -19.49999999982360066, -0.1021026942259700004, -2.500000000000000000 ) ) ;
#18594 = AXIS2_PLACEMENT_3D ( 'NONE', #13602, #20725, #19077 ) ;
#18595 = AXIS2_PLACEMENT_3D ( 'NONE', #10743, #5488, #8944 ) ;
#18596 = DIRECTION ( 'NONE',  ( 3.837966487416234409E-32, -1.188439662295820021E-15, -1.000000000000000000 ) ) ;
#18597 = CIRCLE ( 'NONE', #15548, 2.066999999999999726 ) ;
#18598 = DIRECTION ( 'NONE',  ( 0.000000000000000000, 0.000000000000000000, -1.000000000000000000 ) ) ;
#18599 = EDGE_LOOP ( 'NONE', ( #616, #13150, #21407, #13430, #14033 ) ) ;
#18600 = ORIENTED_EDGE ( 'NONE', *, *, #21881, .F. ) ;
#18601 = FACE_OUTER_BOUND ( 'NONE', #18176, .T. ) ;
#18602 = CARTESIAN_POINT ( 'NONE',  ( 32.77470933150577537, -5.589124729719509688, -13.00000000000039968 ) ) ;
#18603 = ORIENTED_EDGE ( 'NONE', *, *, #19682, .F. ) ;
#18604 = CIRCLE ( 'NONE', #8354, 0.09999999999999999167 ) ;
#18605 = CARTESIAN_POINT ( 'NONE',  ( -0.5391976746782148888, 18.33937061236850141, 3.301631463538509622E-17 ) ) ;
#18606 = EDGE_CURVE ( 'NONE', #8980, #20796, #6557, .T. ) ;
#18607 = EDGE_LOOP ( 'NONE', ( #4462, #20175, #2153, #21701 ) ) ;
#18608 = CARTESIAN_POINT ( 'NONE',  ( -69.90454993788389970, 6.134066389438220135, 3.000000000000100364 ) ) ;
#18609 = APPROVAL_STATUS ( 'not_yet_approved' ) ;
#18610 = CARTESIAN_POINT ( 'NONE',  ( 37.65485242725145554, 9.563919128020760496, -8.996926784497379259 ) ) ;
#18611 = PRODUCT_DEFINITION_SHAPE ( 'NONE', 'NONE',  #23505 ) ;
#18612 = LOCAL_TIME ( 14, 11, 27.00000000000000000, #10364 ) ;
#18613 = DATE_AND_TIME ( #9823, #15996 ) ;
#18614 = DIRECTION ( 'NONE',  ( 0.9730401042858034533, -0.2306359803922031215, 0.000000000000000000 ) ) ;
#18615 = AXIS2_PLACEMENT_3D ( 'NONE', #3861, #20369, #14787 ) ;
#18616 = ORIENTED_EDGE ( 'NONE', *, *, #9954, .T. ) ;
#18617 = DIRECTION ( 'NONE',  ( -1.159535895544890222E-14, -2.167612681253619929E-15, -1.000000000000000000 ) ) ;
#18618 = ORIENTED_EDGE ( 'NONE', *, *, #3622, .F. ) ;
#18620 = AXIS2_PLACEMENT_3D ( 'NONE', #5119, #3330, #7568 ) ;
#18619 = CARTESIAN_POINT ( 'NONE',  ( -17.47493720815329965, 28.95208920939580111, -5.499999999996149747 ) ) ;
#18621 = DIRECTION ( 'NONE',  ( 1.159535895544890222E-14, 2.167612681253619929E-15, 1.000000000000000000 ) ) ;
#18622 = ORIENTED_EDGE ( 'NONE', *, *, #558, .F. ) ;
#18623 = CARTESIAN_POINT ( 'NONE',  ( -66.29618031796869104, -0.3471291603817620031, 5.500000000000099476 ) ) ;
#18624 = DIRECTION ( 'NONE',  ( -0.9997651245102160411, -0.02167246670483410909, 0.000000000000000000 ) ) ;
#18625 = ORIENTED_EDGE ( 'NONE', *, *, #4874, .F. ) ;
#18626 = APPROVAL_PERSON_ORGANIZATION ( #20689, #6938, #16769 ) ;
#18627 = CONTEXT_DEPENDENT_SHAPE_REPRESENTATION ( #13847, #2280 ) ;
#18628 = DIRECTION ( 'NONE',  ( -8.623081276789554834E-17, -1.054188326053478339E-16, -1.000000000000000000 ) ) ;
#18629 = LOCAL_TIME ( 14, 11, 27.00000000000000000, #17497 ) ;
#18630 = EDGE_LOOP ( 'NONE', ( #4511, #12649, #14004, #9294 ) ) ;
#18631 = EDGE_CURVE ( 'NONE', #16326, #9360, #9982, .T. ) ;
#18632 = PERSON_AND_ORGANIZATION_ROLE ( 'creator' ) ;
#18633 = CARTESIAN_POINT ( 'NONE',  ( 30.76933207471829945, -4.221800468112443916, 12.00000000000019185 ) ) ;
#18634 = EDGE_CURVE ( 'NONE', #5198, #13888, #5641, .T. ) ;
#18635 = VERTEX_POINT ( 'NONE', #20137 ) ;
#18636 = ORIENTED_EDGE ( 'NONE', *, *, #5240, .F. ) ;
#18637 = SECURITY_CLASSIFICATION ( '', '', #20985 ) ;
#18638 = FACE_BOUND ( 'NONE', #15388, .T. ) ;
#18639 = PERSON_AND_ORGANIZATION_ROLE ( 'creator' ) ;
#18640 = VECTOR ( 'NONE', #11981, 1000.000000000000000 ) ;
#18641 = CONTEXT_DEPENDENT_SHAPE_REPRESENTATION ( #10857, #6083 ) ;
#18642 = CARTESIAN_POINT ( 'NONE',  ( 43.45766680872420551, 21.27115113520920175, 13.00000000000000000 ) ) ;
#18643 = EDGE_CURVE ( 'NONE', #1017, #17221, #9601, .T. ) ;
#18644 = EDGE_CURVE ( 'NONE', #18495, #18753, #1841, .T. ) ;
#18645 = LOCAL_TIME ( 14, 11, 27.00000000000000000, #14945 ) ;
#18646 =( NAMED_UNIT ( * ) PLANE_ANGLE_UNIT ( ) SI_UNIT ( $, .RADIAN. ) );
#18647 = LOCAL_TIME ( 14, 11, 27.00000000000000000, #21758 ) ;
#18648 = DIRECTION ( 'NONE',  ( 0.2306359803922077290, 0.9730401042858024541, -1.412237191019971018E-17 ) ) ;
#18649 = PERSON_AND_ORGANIZATION ( #11966, #8758 ) ;
#18650 = ORIENTED_EDGE ( 'NONE', *, *, #6517, .T. ) ;
#18651 = CC_DESIGN_APPROVAL ( #5292, ( #1928 ) ) ;
#18652 = DIRECTION ( 'NONE',  ( 1.138590270679731958E-14, 2.220446049251240387E-15, 1.000000000000000000 ) ) ;
#18653 = ORIENTED_EDGE ( 'NONE', *, *, #17108, .T. ) ;
#18654 = DIRECTION ( 'NONE',  ( 1.000000000000000000, -2.270069654138870255E-15, 7.033657510914128686E-46 ) ) ;
#18655 = DIRECTION ( 'NONE',  ( -0.9730401042858035643, 0.2306359803922028717, -2.804983810440357322E-16 ) ) ;
#18656 = CARTESIAN_POINT ( 'NONE',  ( -20.00000000397270128, 22.95208919257159863, 5.000000000004460432 ) ) ;
#18657 = EDGE_LOOP ( 'NONE', ( #17452, #13487, #590, #4569 ) ) ;
#18658 = ORIENTED_EDGE ( 'NONE', *, *, #16871, .T. ) ;
#18659 = LINE ( 'NONE', #13306, #21600 ) ;
#18660 = EDGE_LOOP ( 'NONE', ( #2841, #20911, #20336, #4042 ) ) ;
#18661 = COORDINATED_UNIVERSAL_TIME_OFFSET ( 0, 0, .AHEAD. ) ;
#18662 = EDGE_CURVE ( 'NONE', #19315, #17891, #14887, .T. ) ;
#18663 = CC_DESIGN_SECURITY_CLASSIFICATION ( #9939, ( #16369 ) ) ;
#18664 = EDGE_LOOP ( 'NONE', ( #5531, #19573, #7800, #2452 ) ) ;
#18665 = EDGE_LOOP ( 'NONE', ( #13812, #11893 ) ) ;
#18666 = DIRECTION ( 'NONE',  ( 2.270069654138865127E-15, 1.000000000000000000, 4.574083617919690056E-30 ) ) ;
#18667 = CARTESIAN_POINT ( 'NONE',  ( -22.99995202268987171, -0.1204285676208968203, -8.616475246431379602E-14 ) ) ;
#18668 = PERSON_AND_ORGANIZATION_ROLE ( 'creator' ) ;
#18669 = CIRCLE ( 'NONE', #4616, 0.5000000000000004441 ) ;
#18670 = LINE ( 'NONE', #2388, #21470 ) ;
#18671 = CC_DESIGN_PERSON_AND_ORGANIZATION_ASSIGNMENT ( #16649, #22232, ( #6978 ) ) ;
#18672 = CC_DESIGN_PERSON_AND_ORGANIZATION_ASSIGNMENT ( #5017, #21403, ( #3492 ) ) ;
#18673 = DIRECTION ( 'NONE',  ( 6.123230174520409620E-17, 4.962644601432260272E-15, 1.000000000000000000 ) ) ;
#18674 = LOCAL_TIME ( 14, 11, 27.00000000000000000, #12199 ) ;
#18675 = EDGE_CURVE ( 'NONE', #1138, #2989, #4655, .T. ) ;
#18676 = EDGE_CURVE ( 'NONE', #13601, #16953, #7924, .T. ) ;
#18677 =( NAMED_UNIT ( * ) PLANE_ANGLE_UNIT ( ) SI_UNIT ( $, .RADIAN. ) );
#18678 = ORIENTED_EDGE ( 'NONE', *, *, #22160, .F. ) ;
#18679 = DIRECTION ( 'NONE',  ( 3.099353312215989243E-62, -1.534091707905539548E-92, -1.000000000000000000 ) ) ;
#18680 = SHAPE_DEFINITION_REPRESENTATION ( #16297, #12508 ) ;
#18681 = LOCAL_TIME ( 14, 11, 27.00000000000000000, #2861 ) ;
#18682 = VERTEX_POINT ( 'NONE', #3633 ) ;
#18683 = CARTESIAN_POINT ( 'NONE',  ( 35.24824457160689661, 8.315249525024576371, -27.55602540378494325 ) ) ;
#18684 = VECTOR ( 'NONE', #20094, 1000.000000000000114 ) ;
#18685 = DIRECTION ( 'NONE',  ( -0.9730401042858035643, 0.2306359803922028717, 5.958148513035547083E-17 ) ) ;
#18686 = EDGE_LOOP ( 'NONE', ( #429, #11368, #5903, #9098 ) ) ;
#18687 = VECTOR ( 'NONE', #19102, 1000.000000000000000 ) ;
#18688 = LINE ( 'NONE', #13557, #14297 ) ;
#18689 = CIRCLE ( 'NONE', #8445, 3.499999999999999556 ) ;
#18690 = CARTESIAN_POINT ( 'NONE',  ( 35.11747397072451093, 7.763535785894755570, 19.56700000000001083 ) ) ;
#18691 = ORIENTED_EDGE ( 'NONE', *, *, #10588, .F. ) ;
#18692 = APPROVAL_PERSON_ORGANIZATION ( #13507, #6897, #20639 ) ;
#18693 = CYLINDRICAL_SURFACE ( 'NONE', #82, 2.066999999999998838 ) ;
#18694 = APPROVAL_DATE_TIME ( #22574, #6938 ) ;
#18695 = EDGE_CURVE ( 'NONE', #4801, #23060, #16328, .T. ) ;
#18696 = EDGE_LOOP ( 'NONE', ( #23246, #19128, #20487, #7923 ) ) ;
#18697 = ORIENTED_EDGE ( 'NONE', *, *, #13435, .F. ) ;
#18698 = DIRECTION ( 'NONE',  ( 1.734723475976802677E-14, 9.540979117872415038E-14, -1.000000000000000000 ) ) ;
#18699 = DIRECTION ( 'NONE',  ( -0.02168293463503252055, 0.9997648975362223300, -2.428612866367530721E-15 ) ) ;
#18700 = ORIENTED_EDGE ( 'NONE', *, *, #15162, .T. ) ;
#18701 = PERSON_AND_ORGANIZATION_ROLE ( 'design_supplier' ) ;
#18702 = CARTESIAN_POINT ( 'NONE',  ( 36.98239558567010477, 9.060380560764929925, -29.25000000000050093 ) ) ;
#18703 = CC_DESIGN_APPROVAL ( #10427, ( #6551 ) ) ;
#18704 = DIRECTION ( 'NONE',  ( -0.2306359803922031215, -0.9730401042858033422, 0.000000000000000000 ) ) ;
#18705 = DATE_AND_TIME ( #18823, #4319 ) ;
#18706 = AXIS2_PLACEMENT_3D ( 'NONE', #19155, #8335, #17473 ) ;
#18707 = FACE_OUTER_BOUND ( 'NONE', #3889, .T. ) ;
#18708 = ADVANCED_FACE ( 'NONE', ( #9331, #18369 ), #16447, .T. ) ;
#18709 = VECTOR ( 'NONE', #9932, 1000.000000000000000 ) ;
#18710 = EDGE_CURVE ( 'NONE', #4918, #1609, #14131, .T. ) ;
#18711 = AXIS2_PLACEMENT_3D ( 'NONE', #6005, #13488, #17165 ) ;
#18712 = APPLICATION_CONTEXT ( 'configuration controlled 3d designs of mechanical parts and assemblies' ) ;
#18713 = DIRECTION ( 'NONE',  ( -0.2306359803922084506, -0.9730401042858020100, 5.112869192352694760E-15 ) ) ;
#18714 = AXIS2_PLACEMENT_3D ( 'NONE', #22843, #13834, #17750 ) ;
#18715 = CARTESIAN_POINT ( 'NONE',  ( -62.93867965702761325, 12.67062903583649991, 1.345427500395039956E-15 ) ) ;
#18716 = PERSON_AND_ORGANIZATION ( #11966, #8758 ) ;
#18717 = DIRECTION ( 'NONE',  ( 0.9999862922474493931, 0.005235963827116132258, -1.466966272681990539E-16 ) ) ;
#18718 = VECTOR ( 'NONE', #14703, 1000.000000000000000 ) ;
#18719 = LINE ( 'NONE', #13007, #12456 ) ;
#18720 = AXIS2_PLACEMENT_3D ( 'NONE', #19597, #16142, #7025 ) ;
#18721 = DIRECTION ( 'NONE',  ( -0.07397971354964408275, -0.9972597464969258363, 2.255140518769849223E-15 ) ) ;
#18722 = APPROVAL_PERSON_ORGANIZATION ( #16456, #5163, #5425 ) ;
#18723 = DIRECTION ( 'NONE',  ( 0.2306359803922080343, 0.9730401042858022320, -2.974717104243940401E-15 ) ) ;
#18724 = CARTESIAN_POINT ( 'NONE',  ( -25.29411765129259848, 25.77561860384869874, 8.000000000004520828 ) ) ;
#18725 = AXIS2_PLACEMENT_3D ( 'NONE', #8555, #19232, #22780 ) ;
#18726 = LINE ( 'NONE', #5880, #13001 ) ;
#18727 = AXIS2_PLACEMENT_3D ( 'NONE', #5151, #23071, #6829 ) ;
#18728 = ORIENTED_EDGE ( 'NONE', *, *, #12034, .F. ) ;
#18729 = ADVANCED_BREP_SHAPE_REPRESENTATION ( '', ( #2022, #12739 ), #14020 ) ;
#18730 = ADVANCED_FACE ( 'NONE', ( #21793 ), #13023, .F. ) ;
#18731 = AXIS2_PLACEMENT_3D ( 'NONE', #7298, #14541, #21776 ) ;
#18732 = VERTEX_POINT ( 'NONE', #7437 ) ;
#18733 = FACE_OUTER_BOUND ( 'NONE', #20861, .T. ) ;
#18734 = DIRECTION ( 'NONE',  ( 1.000000000000000000, 9.250447630115842075E-11, -1.144917494144692525E-14 ) ) ;
#18735 = ORIENTED_EDGE ( 'NONE', *, *, #1282, .F. ) ;
#18736 = CARTESIAN_POINT ( 'NONE',  ( 36.12085580342079538, 11.99674675958995174, -19.78350000000001074 ) ) ;
#18737 = VERTEX_POINT ( 'NONE', #11140 ) ;
#18738 = CARTESIAN_POINT ( 'NONE',  ( 59.43368109719860826, 4.124228161845699958, 3.772686752615189359E-14 ) ) ;
#18739 = AXIS2_PLACEMENT_3D ( 'NONE', #3438, #8572, #10363 ) ;
#18740 = APPLICATION_PROTOCOL_DEFINITION ( 'international standard', 'config_control_design', 1994, #14471 ) ;
#18741 = DIRECTION ( 'NONE',  ( 0.000000000000000000, 0.000000000000000000, -1.000000000000000000 ) ) ;
#18742 = EDGE_CURVE ( 'NONE', #18892, #17240, #8063, .T. ) ;
#18743 = SECURITY_CLASSIFICATION ( '', '', #14766 ) ;
#18744 = VECTOR ( 'NONE', #3537, 1000.000000000000227 ) ;
#18745 = EDGE_CURVE ( 'NONE', #5242, #11832, #7323, .T. ) ;
#18746 = APPROVAL_DATE_TIME ( #22264, #10821 ) ;
#18747 =( NAMED_UNIT ( * ) SI_UNIT ( $, .STERADIAN. ) SOLID_ANGLE_UNIT ( ) );
#18748 = VECTOR ( 'NONE', #12036, 1000.000000000000114 ) ;
#18749 = CARTESIAN_POINT ( 'NONE',  ( -14.00000000144870071, -4.350228928435750042, -5.499999999996869171 ) ) ;
#18750 = VERTEX_POINT ( 'NONE', #16669 ) ;
#18751 = CIRCLE ( 'NONE', #9642, 0.9999999999999991118 ) ;
#18752 = LINE ( 'NONE', #22519, #1634 ) ;
#18753 = VERTEX_POINT ( 'NONE', #18016 ) ;
#18754 = DIRECTION ( 'NONE',  ( -1.239096229992449859E-15, -4.969341027244109908E-15, -1.000000000000000000 ) ) ;
#18755 = CARTESIAN_POINT ( 'NONE',  ( 36.68523773071988359, 8.745424676169610834, 27.44000000000022865 ) ) ;
#18756 = ORIENTED_EDGE ( 'NONE', *, *, #5555, .T. ) ;
#18757 = DIRECTION ( 'NONE',  ( 6.123230199561459225E-17, 4.868008300101910084E-15, 1.000000000000000000 ) ) ;
#18758 = FACE_OUTER_BOUND ( 'NONE', #21278, .T. ) ;
#18759 = ORIENTED_EDGE ( 'NONE', *, *, #6028, .T. ) ;
#18760 = AXIS2_PLACEMENT_3D ( 'NONE', #18473, #13356, #18830 ) ;
#18761 = CALENDAR_DATE ( 2026, 31, 10 ) ;
#18762 = CARTESIAN_POINT ( 'NONE',  ( -14.00000000000130029, -19.99999999944489915, -5.499999999996829203 ) ) ;
#18763 = CIRCLE ( 'NONE', #17617, 3.499999999999998224 ) ;
#18764 = VERTEX_POINT ( 'NONE', #8987 ) ;
#18765 = CC_DESIGN_PERSON_AND_ORGANIZATION_ASSIGNMENT ( #3944, #22102, ( #23309 ) ) ;
#18766 = PERSON_AND_ORGANIZATION_ROLE ( 'design_owner' ) ;
#18767 = DIRECTION ( 'NONE',  ( -0.2306359803922032603, -0.9730401042858034533, 0.000000000000000000 ) ) ;
#18768 = ORIENTED_EDGE ( 'NONE', *, *, #7941, .F. ) ;
#18769 = VERTEX_POINT ( 'NONE', #7205 ) ;
#18770 = DIRECTION ( 'NONE',  ( -1.156142442796728099E-15, -6.608067939030890210E-32, 1.000000000000000000 ) ) ;
#18771 = SHAPE_REPRESENTATION ( 'BR-Y-121', ( #21622, #23122, #6844, #21252, #764, #7234, #16683, #12538, #11417, #6459 ), #2286 ) ;
#18772 = DATE_TIME_ROLE ( 'creation_date' ) ;
#18773 = PERSON_AND_ORGANIZATION_ROLE ( 'classification_officer' ) ;
#18774 = DIRECTION ( 'NONE',  ( -0.9730401042858024541, 0.2306359803922080898, 5.959266323858952312E-17 ) ) ;
#18775 = CYLINDRICAL_SURFACE ( 'NONE', #13402, 2.500000000000000444 ) ;
#18776 = EDGE_LOOP ( 'NONE', ( #14289, #3747, #20627, #11577 ) ) ;
#18777 = EDGE_CURVE ( 'NONE', #6701, #21585, #4218, .T. ) ;
#18778 = PERSON_AND_ORGANIZATION ( #11966, #8758 ) ;
#18779 = ORIENTED_EDGE ( 'NONE', *, *, #10452, .F. ) ;
#18780 = CARTESIAN_POINT ( 'NONE',  ( 35.39446192414882120, 8.932132232240713066, -27.19000000000049511 ) ) ;
#18781 = ORIENTED_EDGE ( 'NONE', *, *, #10125, .T. ) ;
#18782 = DIRECTION ( 'NONE',  ( 0.9730401042858035643, -0.2306359803922028717, -5.432877459303547053E-17 ) ) ;
#18783 = CARTESIAN_POINT ( 'NONE',  ( -24.50000000000000000, -28.60000000000000142, 19.00000000000000000 ) ) ;
#18784 = CARTESIAN_POINT ( 'NONE',  ( -20.00000000000000000, -17.50000000000000000, -4.999999999995474731 ) ) ;
#18785 = ORIENTED_EDGE ( 'NONE', *, *, #3171, .T. ) ;
#18786 = ORIENTED_EDGE ( 'NONE', *, *, #21593, .T. ) ;
#18787 = CARTESIAN_POINT ( 'NONE',  ( 33.37436288052550282, -3.059220458576419777, -13.00000000000039968 ) ) ;
#18788 = VERTEX_POINT ( 'NONE', #17031 ) ;
#18789 = PERSON_AND_ORGANIZATION ( #11966, #8758 ) ;
#18790 = ORIENTED_EDGE ( 'NONE', *, *, #4482, .F. ) ;
#18791 = EDGE_LOOP ( 'NONE', ( #19576, #4509 ) ) ;
#18792 = CYLINDRICAL_SURFACE ( 'NONE', #14117, 4.099999999999999645 ) ;
#18793 = APPROVAL_DATE_TIME ( #11564, #5463 ) ;
#18794 = CARTESIAN_POINT ( 'NONE',  ( 34.54155158422950223, 23.97785071899700071, 11.00000000000000000 ) ) ;
#18795 = CIRCLE ( 'NONE', #7406, 2.499999999999998668 ) ;
#18796 = CARTESIAN_POINT ( 'NONE',  ( -20.00000000397369959, 22.95208919256949898, -5.000000000000060396 ) ) ;
#18797 = DIRECTION ( 'NONE',  ( 0.9730401042858036753, -0.2306359803922031493, -8.741838862554654777E-17 ) ) ;
#18798 = EDGE_CURVE ( 'NONE', #7119, #8379, #11886, .T. ) ;
#18799 = DATE_AND_TIME ( #359, #10686 ) ;
#18800 = AXIS2_PLACEMENT_3D ( 'NONE', #11540, #22060, #683 ) ;
#18801 = ORIENTED_EDGE ( 'NONE', *, *, #9969, .F. ) ;
#18802 = CARTESIAN_POINT ( 'NONE',  ( 35.59419854219520118, 9.774809681453278998, 23.00000000000000000 ) ) ;
#18803 = DIRECTION ( 'NONE',  ( -6.662160722082822564E-09, 1.000000000000000000, -2.523234146875356491E-15 ) ) ;
#18804 = ORIENTED_EDGE ( 'NONE', *, *, #15383, .F. ) ;
#18805 = CC_DESIGN_PERSON_AND_ORGANIZATION_ASSIGNMENT ( #20509, #7462, ( #22065 ) ) ;
#18806 = DIRECTION ( 'NONE',  ( -0.9730401042858035643, 0.2306359803922028717, 5.958148513035547083E-17 ) ) ;
#18807 = DIRECTION ( 'NONE',  ( -7.840589463879458156E-32, 2.441916418604790135E-15, 1.000000000000000000 ) ) ;
#18808 = ORIENTED_EDGE ( 'NONE', *, *, #17625, .F. ) ;
#18809 = DIRECTION ( 'NONE',  ( 0.2306359803922080343, 0.9730401042858022320, 5.907067092757291018E-15 ) ) ;
#18810 = EDGE_CURVE ( 'NONE', #3926, #14730, #19825, .T. ) ;
#18811 = EDGE_CURVE ( 'NONE', #16103, #19758, #21712, .T. ) ;
#18812 = PERSON_AND_ORGANIZATION ( #11966, #8758 ) ;
#18813 = PRODUCT_DEFINITION_SHAPE ( 'NONE', 'NONE',  #23510 ) ;
#18814 = ORIENTED_EDGE ( 'NONE', *, *, #7481, .T. ) ;
#18815 = VERTEX_POINT ( 'NONE', #7663 ) ;
#18816 = DIRECTION ( 'NONE',  ( 1.000000000000000000, -1.555753819465284865E-62, -8.326672684687908612E-17 ) ) ;
#18817 = DIRECTION ( 'NONE',  ( 0.005235963827108352890, -0.9999862922474493931, -5.936218956694023463E-19 ) ) ;
#18818 = ORIENTED_EDGE ( 'NONE', *, *, #16814, .F. ) ;
#18819 = DATE_AND_TIME ( #727, #9173 ) ;
#18820 = CARTESIAN_POINT ( 'NONE',  ( -1.692377576641375780, 13.47417009093944174, -8.163194603328985906E-15 ) ) ;
#18821 = CIRCLE ( 'NONE', #3999, 2.499999999999998668 ) ;
#18822 = CARTESIAN_POINT ( 'NONE',  ( -18.05391955182270181, 22.49081825942809942, 2.500000000000000000 ) ) ;
#18823 = CALENDAR_DATE ( 2026, 31, 10 ) ;
#18824 = DIRECTION ( 'NONE',  ( -0.9999862922474492821, -0.005235963827121951387, 1.239088197126291310E-16 ) ) ;
#18825 = CIRCLE ( 'NONE', #3631, 2.500000000000000000 ) ;
#18826 = CARTESIAN_POINT ( 'NONE',  ( -19.49999999982360066, -0.1021026942259579962, 5.000000000000000000 ) ) ;
#18827 = ADVANCED_FACE ( 'NONE', ( #18843, #13245, #13596 ), #22603, .T. ) ;
#18828 = CALENDAR_DATE ( 2026, 31, 10 ) ;
#18829 =( BOUNDED_CURVE ( )  B_SPLINE_CURVE ( 2, ( #15012, #16797, #8016 ),
 .UNSPECIFIED., .F., .F. ) 
 B_SPLINE_CURVE_WITH_KNOTS ( ( 3, 3 ),
 ( 0.000000000000000000, 0.1752654207116860208 ),
 .UNSPECIFIED. ) 
 CURVE ( )  GEOMETRIC_REPRESENTATION_ITEM ( )  RATIONAL_B_SPLINE_CURVE ( ( 1.000000000000000000, 1.154700538379249908, 1.000000000000000000 ) ) 
 REPRESENTATION_ITEM ( '' )  );
#18830 = DIRECTION ( 'NONE',  ( 0.000000000000000000, -1.000000000000000000, 0.000000000000000000 ) ) ;
#18831 = DIRECTION ( 'NONE',  ( -0.9730401042858035643, 0.2306359803922028717, 6.126766849694256332E-17 ) ) ;
#18832 = CC_DESIGN_PERSON_AND_ORGANIZATION_ASSIGNMENT ( #13061, #2353, ( #1997 ) ) ;
#18833 = DIRECTION ( 'NONE',  ( -6.662160722082822564E-09, 1.000000000000000000, -2.523234146875356491E-15 ) ) ;
#18834 = DIRECTION ( 'NONE',  ( -2.920245690604589998E-14, -1.234618914536939803E-13, 1.000000000000000000 ) ) ;
#18835 = CC_DESIGN_PERSON_AND_ORGANIZATION_ASSIGNMENT ( #13678, #10491, ( #7614 ) ) ;
#18836 = DIRECTION ( 'NONE',  ( 0.6988463228792121118, 0.7152718483193672983, 1.371062488412534409E-16 ) ) ;
#18837 = ADVANCED_FACE ( 'NONE', ( #18601 ), #10355, .T. ) ;
#18839 = ORIENTED_EDGE ( 'NONE', *, *, #17234, .T. ) ;
#18838 = ADVANCED_FACE ( 'NONE', ( #18733 ), #2447, .T. ) ;
#18840 = CONICAL_SURFACE ( 'NONE', #217, 1.154700538379250796, 1.047197551196598297 ) ;
#18841 = CC_DESIGN_DATE_AND_TIME_ASSIGNMENT ( #14830, #450, ( #6843 ) ) ;
#18842 = ORIENTED_EDGE ( 'NONE', *, *, #6646, .T. ) ;
#18843 = FACE_BOUND ( 'NONE', #21011, .T. ) ;
#18844 = ORIENTED_EDGE ( 'NONE', *, *, #21307, .T. ) ;
#18845 = LINE ( 'NONE', #15376, #5055 ) ;
#18846 = ORIENTED_EDGE ( 'NONE', *, *, #1038, .F. ) ;
#18847 = CARTESIAN_POINT ( 'NONE',  ( 37.48968750243700043, 22.68571848161329996, 13.00000000000000000 ) ) ;
#18848 = APPROVAL_STATUS ( 'not_yet_approved' ) ;
#18849 = CARTESIAN_POINT ( 'NONE',  ( -20.00000000000000000, -15.00000000000000000, -4.999999999995480060 ) ) ;
#18850 = AXIS2_PLACEMENT_3D ( 'NONE', #21748, #5485, #3695 ) ;
#18851 = APPROVAL_DATE_TIME ( #18957, #18067 ) ;
#18852 = AXIS2_PLACEMENT_3D ( 'NONE', #247, #6170, #13424 ) ;
#18853 = CARTESIAN_POINT ( 'NONE',  ( -20.00000000000000000, -20.00000000000000000, -4.999999999995470290 ) ) ;
#18854 = EDGE_CURVE ( 'NONE', #15831, #12377, #13366, .T. ) ;
#18855 = CARTESIAN_POINT ( 'NONE',  ( 102.3363885986873356, 5.191082435725835609, 13.00000000000000000 ) ) ;
#18856 = ORIENTED_EDGE ( 'NONE', *, *, #20028, .F. ) ;
#18857 = LINE ( 'NONE', #7684, #4883 ) ;
#18858 = EDGE_CURVE ( 'NONE', #23125, #15635, #20368, .T. ) ;
#18859 = CARTESIAN_POINT ( 'NONE',  ( 32.80472184429622473, 19.68535052198753377, -2.008708621733521550E-15 ) ) ;
#18860 = EDGE_LOOP ( 'NONE', ( #9736, #9972, #2034, #15399, #18070 ) ) ;
#18861 = CARTESIAN_POINT ( 'NONE',  ( -62.93867965702758482, 12.67062903583649991, 2.999765877365342615 ) ) ;
#18862 = CARTESIAN_POINT ( 'NONE',  ( 121.3909450504253584, 5.368190954742520837, 13.00000000000000000 ) ) ;
#18863 = ORIENTED_EDGE ( 'NONE', *, *, #7623, .T. ) ;
#18864 = ADVANCED_FACE ( 'NONE', ( #748 ), #8023, .T. ) ;
#18865 = AXIS2_PLACEMENT_3D ( 'NONE', #4478, #904, #9726 ) ;
#18866 = APPROVAL_STATUS ( 'not_yet_approved' ) ;
#18867 = EDGE_CURVE ( 'NONE', #22209, #1782, #17164, .T. ) ;
#18868 = DIRECTION ( 'NONE',  ( -0.04564792618500997101, -0.9989575901083128651, 2.775557561562890562E-15 ) ) ;
#18869 = ORIENTED_EDGE ( 'NONE', *, *, #1057, .F. ) ;
#18870 = APPROVAL_DATE_TIME ( #784, #17220 ) ;
#18871 = DIRECTION ( 'NONE',  ( -5.964507377817349415E-17, -4.861311874385510251E-15, -1.000000000000000000 ) ) ;
#18872 = ORIENTED_EDGE ( 'NONE', *, *, #2425, .F. ) ;
#18873 = ORIENTED_EDGE ( 'NONE', *, *, #12424, .F. ) ;
#18874 = VECTOR ( 'NONE', #23196, 1000.000000000000000 ) ;
#18875 = SECURITY_CLASSIFICATION_LEVEL ( 'unclassified' ) ;
#18876 = APPROVAL_DATE_TIME ( #11404, #4295 ) ;
#18877 = AXIS2_PLACEMENT_3D ( 'NONE', #18089, #1570, #20092 ) ;
#18878 = CARTESIAN_POINT ( 'NONE',  ( 58.25686728443099582, 17.76335315678740301, -13.00000000000049916 ) ) ;
#18879 = AXIS2_PLACEMENT_3D ( 'NONE', #18584, #2431, #16786 ) ;
#18880 = CIRCLE ( 'NONE', #3322, 15.25000000000000000 ) ;
#18881 = DIRECTION ( 'NONE',  ( 0.000000000000000000, 0.000000000000000000, -1.000000000000000000 ) ) ;
#18882 = VERTEX_POINT ( 'NONE', #7901 ) ;
#18883 = APPROVAL_DATE_TIME ( #20651, #18236 ) ;
#18884 = ORIENTED_EDGE ( 'NONE', *, *, #18512, .F. ) ;
#18885 = DIRECTION ( 'NONE',  ( 0.000000000000000000, 0.000000000000000000, -1.000000000000000000 ) ) ;
#18886 = FACE_OUTER_BOUND ( 'NONE', #7268, .T. ) ;
#18887 = ORIENTED_EDGE ( 'NONE', *, *, #9674, .F. ) ;
#18888 = LINE ( 'NONE', #16972, #679 ) ;
#18889 = CARTESIAN_POINT ( 'NONE',  ( 96.81657767996070163, -18.09668638014640152, 13.00000000000000000 ) ) ;
#18890 = CARTESIAN_POINT ( 'NONE',  ( -28.52462712253550237, 6.350733138482030249, -0.7325259402521649976 ) ) ;
#18891 = AXIS2_PLACEMENT_3D ( 'NONE', #16385, #7487, #11065 ) ;
#18892 = VERTEX_POINT ( 'NONE', #15131 ) ;
#18893 = ORIENTED_EDGE ( 'NONE', *, *, #1252, .F. ) ;
#18894 = CARTESIAN_POINT ( 'NONE',  ( 6.748807626790974012, 18.73619264518185901, -5.433717567020060490E-15 ) ) ;
#18895 = EDGE_LOOP ( 'NONE', ( #17962, #7841 ) ) ;
#18896 = CALENDAR_DATE ( 2026, 31, 10 ) ;
#18897 = VECTOR ( 'NONE', #21785, 999.9999999999998863 ) ;
#18898 = VERTEX_POINT ( 'NONE', #22369 ) ;
#18899 = ORIENTED_EDGE ( 'NONE', *, *, #22689, .T. ) ;
#18900 = LINE ( 'NONE', #9874, #23210 ) ;
#18901 = AXIS2_PLACEMENT_3D ( 'NONE', #18826, #15119, #6231 ) ;
#18902 = PERSON_AND_ORGANIZATION ( #11966, #8758 ) ;
#18903 = DIRECTION ( 'NONE',  ( 0.9730401042858035643, -0.2306359803922028717, -5.958148513035547083E-17 ) ) ;
#18904 = EDGE_CURVE ( 'NONE', #1573, #4918, #4563, .T. ) ;
#18905 = FACE_OUTER_BOUND ( 'NONE', #14763, .T. ) ;
#18906 = AXIS2_PLACEMENT_3D ( 'NONE', #5779, #7799, #22517 ) ;
#18907 = CARTESIAN_POINT ( 'NONE',  ( 36.30795141656454916, -8.893092097652150585, -18.00000000000000000 ) ) ;
#18908 = APPROVAL_STATUS ( 'not_yet_approved' ) ;
#18909 = AXIS2_PLACEMENT_3D ( 'NONE', #4551, #3123, #18933 ) ;
#18910 = ORIENTED_EDGE ( 'NONE', *, *, #15123, .T. ) ;
#18911 = CYLINDRICAL_SURFACE ( 'NONE', #15939, 3.499999999999999556 ) ;
#18912 = DIRECTION ( 'NONE',  ( -0.9730401042858023430, 0.2306359803922080620, 5.959266323858944916E-17 ) ) ;
#18913 = ORIENTED_EDGE ( 'NONE', *, *, #16743, .F. ) ;
#18914 = LINE ( 'NONE', #4180, #22252 ) ;
#18915 = DIRECTION ( 'NONE',  ( -0.9730401042858022320, 0.2306359803922080343, 5.959266323858941219E-17 ) ) ;
#18916 = ORIENTED_EDGE ( 'NONE', *, *, #13877, .F. ) ;
#18917 = FACE_OUTER_BOUND ( 'NONE', #15887, .T. ) ;
#18918 = APPROVAL_ROLE ( '' ) ;
#18919 = ORIENTED_EDGE ( 'NONE', *, *, #13921, .F. ) ;
#18920 = ORIENTED_EDGE ( 'NONE', *, *, #11599, .F. ) ;
#18921 = CARTESIAN_POINT ( 'NONE',  ( 31.11077410011089839, -1.335996977273280262, -15.00000000000039968 ) ) ;
#18922 = FACE_OUTER_BOUND ( 'NONE', #16880, .T. ) ;
#18923 = ORIENTED_EDGE ( 'NONE', *, *, #19548, .T. ) ;
#18924 = PERSON_AND_ORGANIZATION ( #11966, #8758 ) ;
#18925 = CARTESIAN_POINT ( 'NONE',  ( 43.81210844073630994, 9.047859270861110303, -21.50000000000000000 ) ) ;
#18926 = EDGE_CURVE ( 'NONE', #23261, #10381, #9198, .T. ) ;
#18927 = CARTESIAN_POINT ( 'NONE',  ( 0.000000000000000000, -3.886126572655959799E-16, -2.500000000000000000 ) ) ;
#18928 = AXIS2_PLACEMENT_3D ( 'NONE', #3810, #2042, #9290 ) ;
#18929 = CALENDAR_DATE ( 2026, 31, 10 ) ;
#18930 = DIRECTION ( 'NONE',  ( -1.187319687680499994E-16, -2.805478249478695031E-20, -1.000000000000000000 ) ) ;
#18931 = ADVANCED_FACE ( 'NONE', ( #20613 ), #6243, .T. ) ;
#18932 = EDGE_CURVE ( 'NONE', #17128, #2498, #16023, .T. ) ;
#18933 = DIRECTION ( 'NONE',  ( 0.9949874374308176339, 0.09999999677427344469, -2.262079412673755946E-13 ) ) ;
#18934 = APPROVAL_STATUS ( 'not_yet_approved' ) ;
#18935 = DIRECTION ( 'NONE',  ( 1.000000000000000000, 9.794583108699330061E-17, 0.000000000000000000 ) ) ;
#18936 = FACE_OUTER_BOUND ( 'NONE', #3481, .T. ) ;
#18937 = CARTESIAN_POINT ( 'NONE',  ( -17.50034580627744063, 23.00627559326238369, 3.749999999999900080 ) ) ;
#18938 = EDGE_CURVE ( 'NONE', #15497, #16018, #15656, .T. ) ;
#18939 = CARTESIAN_POINT ( 'NONE',  ( -19.63010143622448211, 27.93838792505352941, -4.999999999995571542 ) ) ;
#18940 = FACE_OUTER_BOUND ( 'NONE', #7265, .T. ) ;
#18941 = CARTESIAN_POINT ( 'NONE',  ( -20.00000000000000000, -17.50000000000000000, 5.000000000004554579 ) ) ;
#18942 = ORIENTED_EDGE ( 'NONE', *, *, #17997, .T. ) ;
#18943 = VERTEX_POINT ( 'NONE', #5046 ) ;
#18944 = DIRECTION ( 'NONE',  ( -2.269747459788999852E-13, -2.220446049250325308E-15, -1.000000000000000000 ) ) ;
#18945 = CYLINDRICAL_SURFACE ( 'NONE', #14377, 2.500000000000000444 ) ;
#18946 = ORGANIZATION ( 'NAUO-ORG13', 'UNSPECIFIED', 'UNSPECIFIED' ) ;
#18947 = ORIENTED_EDGE ( 'NONE', *, *, #3530, .F. ) ;
#18948 = CIRCLE ( 'NONE', #8709, 2.500000000000000444 ) ;
#18949 = FACE_BOUND ( 'NONE', #22572, .T. ) ;
#18950 = ADVANCED_FACE ( 'NONE', ( #4803 ), #8721, .F. ) ;
#18951 = VERTEX_POINT ( 'NONE', #20951 ) ;
#18952 = DIRECTION ( 'NONE',  ( 0.000000000000000000, 0.000000000000000000, -1.000000000000000000 ) ) ;
#18953 = DATE_TIME_ROLE ( 'classification_date' ) ;
#18954 = DIRECTION ( 'NONE',  ( -2.269747459788990007E-13, -2.220446049250330436E-15, -1.000000000000000000 ) ) ;
#18955 = CC_DESIGN_PERSON_AND_ORGANIZATION_ASSIGNMENT ( #18140, #16115, ( #14534 ) ) ;
#18956 = CC_DESIGN_PERSON_AND_ORGANIZATION_ASSIGNMENT ( #2288, #13113, ( #6898 ) ) ;
#18957 = DATE_AND_TIME ( #6253, #18276 ) ;
#18958 = CARTESIAN_POINT ( 'NONE',  ( -20.00000000397369959, 22.95208919256949898, -5.000000000000060396 ) ) ;
#18959 = EDGE_CURVE ( 'NONE', #638, #5825, #73, .T. ) ;
#18960 = EDGE_CURVE ( 'NONE', #2561, #22329, #7787, .T. ) ;
#18961 = EDGE_CURVE ( 'NONE', #16110, #131, #10286, .T. ) ;
#18962 = VECTOR ( 'NONE', #19534, 999.9999999999998863 ) ;
#18963 = CARTESIAN_POINT ( 'NONE',  ( 30.31182762792540331, -4.706706774123539994, -13.00000000000039968 ) ) ;
#18964 = AXIS2_PLACEMENT_3D ( 'NONE', #14840, #9508, #11558 ) ;
#18965 = ORIENTED_EDGE ( 'NONE', *, *, #3297, .F. ) ;
#18966 = CARTESIAN_POINT ( 'NONE',  ( -20.00000000000000000, -20.00000000000000000, 5.500000000004559020 ) ) ;
#18967 = FACE_OUTER_BOUND ( 'NONE', #19259, .T. ) ;
#18968 = ORIENTED_EDGE ( 'NONE', *, *, #13562, .F. ) ;
#18969 = AXIS2_PLACEMENT_3D ( 'NONE', #4796, #15602, #20943 ) ;
#18970 = DIRECTION ( 'NONE',  ( -0.9730401042858022320, 0.2306359803922080343, 5.959266323858941219E-17 ) ) ;
#18971 = CYLINDRICAL_SURFACE ( 'NONE', #23165, 2.500000000000000000 ) ;
#18972 = DIRECTION ( 'NONE',  ( -0.9997651245880592175, -0.02167246311387460711, 0.000000000000000000 ) ) ;
#18973 = EDGE_LOOP ( 'NONE', ( #9551, #10132, #23281, #18804, #21117, #17455, #11167, #4854, #6469 ) ) ;
#18974 = PERSON_AND_ORGANIZATION_ROLE ( 'classification_officer' ) ;
#18975 = LINE ( 'NONE', #785, #1984 ) ;
#18976 = EDGE_CURVE ( 'NONE', #14619, #13456, #19184, .T. ) ;
#18977 = ORIENTED_EDGE ( 'NONE', *, *, #22294, .T. ) ;
#18978 = LOCAL_TIME ( 14, 11, 27.00000000000000000, #4619 ) ;
#18979 = ORIENTED_EDGE ( 'NONE', *, *, #10961, .T. ) ;
#18980 = APPROVAL_PERSON_ORGANIZATION ( #20561, #6543, #15563 ) ;
#18981 = PERSON_AND_ORGANIZATION ( #11966, #8758 ) ;
#18982 = VECTOR ( 'NONE', #22848, 1000.000000000000000 ) ;
#18983 = APPROVAL_STATUS ( 'not_yet_approved' ) ;
#18984 = DIRECTION ( 'NONE',  ( 6.123230174520370177E-17, 4.962644601432260272E-15, 1.000000000000000000 ) ) ;
#18985 = CIRCLE ( 'NONE', #16310, 2.499999999999999112 ) ;
#18986 = EDGE_CURVE ( 'NONE', #20160, #483, #21182, .T. ) ;
#18987 = EDGE_CURVE ( 'NONE', #10223, #4119, #8257, .T. ) ;
#18988 = VECTOR ( 'NONE', #14629, 999.9999999999998863 ) ;
#18989 = PLANE ( 'NONE',  #21346 ) ;
#18990 = ORIENTED_EDGE ( 'NONE', *, *, #17655, .F. ) ;
#18991 = APPROVAL_DATE_TIME ( #6166, #16346 ) ;
#18992 = PRODUCT_DEFINITION_SHAPE ( 'NONE', 'NONE',  #1530 ) ;
#18993 = CC_DESIGN_APPROVAL ( #16341, ( #22008 ) ) ;
#18994 = ORIENTED_EDGE ( 'NONE', *, *, #3873, .T. ) ;
#18995 = LOCAL_TIME ( 14, 11, 27.00000000000000000, #2302 ) ;
#18996 = DIRECTION ( 'NONE',  ( 1.138590270679731958E-14, 2.220446049251245514E-15, 1.000000000000000000 ) ) ;
#18997 = PLANE ( 'NONE',  #6726 ) ;
#18998 = EDGE_LOOP ( 'NONE', ( #3710, #3489, #1261, #4887 ) ) ;
#18999 = CARTESIAN_POINT ( 'NONE',  ( -27.00000000000000000, -27.34999999999999787, -5.000000000000000000 ) ) ;
#19000 = CARTESIAN_POINT ( 'NONE',  ( -62.73971250800079957, -25.32895006819559924, -5.538452170245418869E-15 ) ) ;
#19001 = DIRECTION ( 'NONE',  ( -0.2306359803922031770, -0.9730401042858034533, 0.000000000000000000 ) ) ;
#19002 = ORIENTED_EDGE ( 'NONE', *, *, #10678, .F. ) ;
#19003 = ORIENTED_EDGE ( 'NONE', *, *, #2427, .T. ) ;
#19004 = CARTESIAN_POINT ( 'NONE',  ( 39.30621916166446539, 3.756429258064753807, 3.834721291928176309E-14 ) ) ;
#19005 = EDGE_LOOP ( 'NONE', ( #4527, #1639, #10366, #23148 ) ) ;
#19006 = VECTOR ( 'NONE', #19095, 999.9999999999998863 ) ;
#19007 = APPROVAL_DATE_TIME ( #818, #21860 ) ;
#19008 = ADVANCED_BREP_SHAPE_REPRESENTATION ( '', ( #1464, #12739 ), #15185 ) ;
#19009 = EDGE_CURVE ( 'NONE', #9430, #11527, #10414, .T. ) ;
#19010 = VERTEX_POINT ( 'NONE', #12186 ) ;
#19011 = VERTEX_POINT ( 'NONE', #8374 ) ;
#19012 = CARTESIAN_POINT ( 'NONE',  ( 34.49867763533220710, 5.152869186095979437, 26.50000000000002487 ) ) ;
#19013 = APPROVAL_DATE_TIME ( #5944, #9224 ) ;
#19014 = CLOSED_SHELL ( 'NONE', ( #7538, #10699, #18560, #21266 ) ) ;
#19015 = CC_DESIGN_SECURITY_CLASSIFICATION ( #10683, ( #8400 ) ) ;
#19016 = CARTESIAN_POINT ( 'NONE',  ( 59.43368109719860826, 4.124228161845699958, 3.772686752615189359E-14 ) ) ;
#19017 = EDGE_CURVE ( 'NONE', #544, #18183, #15490, .T. ) ;
#19018 = CC_DESIGN_APPROVAL ( #11056, ( #14461 ) ) ;
#19019 = EDGE_CURVE ( 'NONE', #11763, #14219, #23189, .T. ) ;
#19020 = CIRCLE ( 'NONE', #3826, 6.000000000001509015 ) ;
#19021 = SHAPE_REPRESENTATION_RELATIONSHIP ( 'NONE' , 'NONE' ,  #15964, #2856 ) ;
#19022 = APPROVAL_PERSON_ORGANIZATION ( #4961, #4117, #10454 ) ;
#19023 = AXIS2_PLACEMENT_3D ( 'NONE', #742, #2789, #17153 ) ;
#19024 = FACE_OUTER_BOUND ( 'NONE', #8774, .T. ) ;
#19025 = APPROVAL_DATE_TIME ( #15442, #6543 ) ;
#19026 = ORIENTED_EDGE ( 'NONE', *, *, #21896, .F. ) ;
#19027 = DIRECTION ( 'NONE',  ( -2.972463603623604872E-47, -1.000000000000000000, -2.972463603623604872E-47 ) ) ;
#19028 = DIRECTION ( 'NONE',  ( 0.9730401042858024541, -0.2306359803922080898, -5.959266323858232476E-17 ) ) ;
#19029 = ORIENTED_EDGE ( 'NONE', *, *, #8643, .F. ) ;
#19030 = APPROVAL_PERSON_ORGANIZATION ( #7208, #20093, #5419 ) ;
#19031 = FACE_OUTER_BOUND ( 'NONE', #21809, .T. ) ;
#19032 = DIRECTION ( 'NONE',  ( 0.000000000000000000, 1.000000000000000000, -9.605990953944227443E-124 ) ) ;
#19033 = SECURITY_CLASSIFICATION ( '', '', #10099 ) ;
#19034 = ORIENTED_EDGE ( 'NONE', *, *, #2113, .T. ) ;
#19035 = CYLINDRICAL_SURFACE ( 'NONE', #4643, 0.4000000000000010214 ) ;
#19036 = AXIS2_PLACEMENT_3D ( 'NONE', #7593, #5930, #2125 ) ;
#19037 = AXIS2_PLACEMENT_3D ( 'NONE', #16166, #21160, #17730 ) ;
#19038 = APPROVAL_DATE_TIME ( #11804, #21286 ) ;
#19039 = EDGE_LOOP ( 'NONE', ( #22371, #7563 ) ) ;
#19040 = ORIENTED_EDGE ( 'NONE', *, *, #12065, .T. ) ;
#19041 = DIRECTION ( 'NONE',  ( -1.187319687680494078E-16, -2.805478249478340539E-20, -1.000000000000000000 ) ) ;
#19042 = CARTESIAN_POINT ( 'NONE',  ( -19.49999999982360066, -0.1021026942259609938, 3.750000000000000000 ) ) ;
#19043 = ORIENTED_EDGE ( 'NONE', *, *, #14829, .F. ) ;
#19044 = ORIENTED_EDGE ( 'NONE', *, *, #3676, .F. ) ;
#19045 = COORDINATED_UNIVERSAL_TIME_OFFSET ( 0, 0, .AHEAD. ) ;
#19046 = PRODUCT_RELATED_PRODUCT_CATEGORY ( 'detail', '', ( #3013 ) ) ;
#19047 = DIRECTION ( 'NONE',  ( 0.2306359803922094498, 0.9730401042858018990, 0.000000000000000000 ) ) ;
#19048 = ADVANCED_FACE ( 'NONE', ( #17639 ), #21070, .F. ) ;
#19049 = CARTESIAN_POINT ( 'NONE',  ( 118.4388045014059969, -7.086722380115170417, -18.89999999999999858 ) ) ;
#19050 = COORDINATED_UNIVERSAL_TIME_OFFSET ( 0, 0, .AHEAD. ) ;
#19051 = LINE ( 'NONE', #4679, #14301 ) ;
#19052 = APPROVAL_PERSON_ORGANIZATION ( #21747, #10684, #20077 ) ;
#19053 = AXIS2_PLACEMENT_3D ( 'NONE', #1987, #9244, #7457 ) ;
#19054 = CARTESIAN_POINT ( 'NONE',  ( 35.59419854219520118, 9.774809681453550780, 27.18999999999999773 ) ) ;
#19055 = DATE_TIME_ROLE ( 'classification_date' ) ;
#19056 = AXIS2_PLACEMENT_3D ( 'NONE', #14946, #8819, #13167 ) ;
#19057 = APPROVAL_PERSON_ORGANIZATION ( #9961, #15302, #17196 ) ;
#19058 = CYLINDRICAL_SURFACE ( 'NONE', #9890, 2.500000000000000000 ) ;
#19059 = DIRECTION ( 'NONE',  ( -0.9730401042858022320, 0.2306359803922080343, 5.959266323858941219E-17 ) ) ;
#19060 = DIRECTION ( 'NONE',  ( 0.9730401042858035643, -0.2306359803922028717, -5.958148513035547083E-17 ) ) ;
#19061 = EDGE_CURVE ( 'NONE', #19614, #19233, #6958, .T. ) ;
#19062 = LINE ( 'NONE', #15013, #26 ) ;
#19063 = AXIS2_PLACEMENT_3D ( 'NONE', #5699, #19860, #3462 ) ;
#19064 = LINE ( 'NONE', #15840, #6917 ) ;
#19065 = DIRECTION ( 'NONE',  ( -0.02167246311338769799, 0.9997651245880698756, -2.441989331389200018E-15 ) ) ;
#19066 = ORIENTED_EDGE ( 'NONE', *, *, #13990, .F. ) ;
#19067 = APPROVAL_PERSON_ORGANIZATION ( #2480, #14898, #4378 ) ;
#19068 = ORIENTED_EDGE ( 'NONE', *, *, #738, .T. ) ;
#19069 = DIRECTION ( 'NONE',  ( -1.448479254059754007E-17, -0.7167018829406569536, 0.6973796749184170141 ) ) ;
#19070 = CARTESIAN_POINT ( 'NONE',  ( -16.50000000144740042, -4.350228928666989958, 6.750000000004490630 ) ) ;
#19071 = ORIENTED_EDGE ( 'NONE', *, *, #15631, .F. ) ;
#19072 = EDGE_CURVE ( 'NONE', #5730, #17119, #22461, .T. ) ;
#19073 = AXIS2_PLACEMENT_3D ( 'NONE', #5884, #11614, #5999 ) ;
#19074 = FACE_OUTER_BOUND ( 'NONE', #11943, .T. ) ;
#19075 = VERTEX_POINT ( 'NONE', #14187 ) ;
#19076 = AXIS2_PLACEMENT_3D ( 'NONE', #1113, #19531, #19646 ) ;
#19077 = DIRECTION ( 'NONE',  ( 0.000000000000000000, -1.000000000000000000, 2.081668171172169697E-15 ) ) ;
#19078 = COORDINATED_UNIVERSAL_TIME_OFFSET ( 0, 0, .AHEAD. ) ;
#19079 = DIRECTION ( 'NONE',  ( -0.9730401042858022320, 0.2306359803922080343, 5.959266323858941219E-17 ) ) ;
#19080 = CIRCLE ( 'NONE', #22091, 6.500000000000000000 ) ;
#19081 = ITEM_DEFINED_TRANSFORMATION ( 'NONE', 'NONE', #2649,  #12739 ) ;
#19082 = CARTESIAN_POINT ( 'NONE',  ( 0.000000000000000000, 0.000000000000000000, 0.000000000000000000 ) ) ;
#19083 = CIRCLE ( 'NONE', #19834, 2.500000000000000444 ) ;
#19085 = LINE ( 'NONE', #2810, #10014 ) ;
#19084 = VECTOR ( 'NONE', #21833, 1000.000000000000114 ) ;
#19086 = DIRECTION ( 'NONE',  ( 4.063875459488300452E-16, -1.011971878839181895E-16, -1.000000000000000000 ) ) ;
#19087 = PRODUCT_DEFINITION_FORMATION_WITH_SPECIFIED_SOURCE ( 'ANY', '', #4576, .NOT_KNOWN. ) ;
#19088 = DIRECTION ( 'NONE',  ( -0.02168293463503252055, 0.9997648975362223300, -2.428612866367530721E-15 ) ) ;
#19089 = AXIS2_PLACEMENT_3D ( 'NONE', #583, #2129, #9388 ) ;
#19090 = ORIENTED_EDGE ( 'NONE', *, *, #2742, .F. ) ;
#19091 = FACE_OUTER_BOUND ( 'NONE', #10504, .T. ) ;
#19092 = VECTOR ( 'NONE', #20343, 999.9999999999997726 ) ;
#19093 = EDGE_CURVE ( 'NONE', #489, #13437, #13782, .T. ) ;
#19094 = AXIS2_PLACEMENT_3D ( 'NONE', #19994, #18215, #16645 ) ;
#19095 = DIRECTION ( 'NONE',  ( 0.9730401042858036753, -0.2306359803922028995, -5.432877459303547669E-17 ) ) ;
#19096 = ORIENTED_EDGE ( 'NONE', *, *, #22385, .T. ) ;
#19097 = LINE ( 'NONE', #20634, #19612 ) ;
#19098 = CARTESIAN_POINT ( 'NONE',  ( -16.00004797695772751, -0.08377682083104273647, -2.500000000000090594 ) ) ;
#19099 = CC_DESIGN_PERSON_AND_ORGANIZATION_ASSIGNMENT ( #11296, #19944, ( #18177 ) ) ;
#19100 = DATE_TIME_ROLE ( 'classification_date' ) ;
#19101 = CC_DESIGN_PERSON_AND_ORGANIZATION_ASSIGNMENT ( #17731, #6928, ( #5761 ) ) ;
#19102 = DIRECTION ( 'NONE',  ( -6.123230199561459225E-17, -4.868008300101910084E-15, -1.000000000000000000 ) ) ;
#19103 = ORIENTED_EDGE ( 'NONE', *, *, #5747, .T. ) ;
#19104 = VECTOR ( 'NONE', #10710, 1000.000000000000000 ) ;
#19105 = ORIENTED_EDGE ( 'NONE', *, *, #14311, .T. ) ;
#19106 = ADVANCED_FACE ( 'NONE', ( #10520 ), #14060, .T. ) ;
#19107 = ADVANCED_FACE ( 'NONE', ( #12409 ), #12654, .F. ) ;
#19108 = APPROVAL_STATUS ( 'not_yet_approved' ) ;
#19109 = DIRECTION ( 'NONE',  ( -0.005235963827108362431, 0.9999862922474493931, 5.936218956694023463E-19 ) ) ;
#19110 = CC_DESIGN_APPROVAL ( #2538, ( #6956 ) ) ;
#19111 = VERTEX_POINT ( 'NONE', #6464 ) ;
#19112 = CARTESIAN_POINT ( 'NONE',  ( 105.3404740731333078, -22.24134309433305390, -13.00000000000000000 ) ) ;
#19113 = PERSON_AND_ORGANIZATION ( #11966, #8758 ) ;
#19114 = VECTOR ( 'NONE', #9210, 999.9999999999998863 ) ;
#19115 = CIRCLE ( 'NONE', #22892, 2.500000000000000444 ) ;
#19116 = COORDINATED_UNIVERSAL_TIME_OFFSET ( 0, 0, .AHEAD. ) ;
#19117 = DIRECTION ( 'NONE',  ( 0.9949874374308235181, 0.09999999677421511635, -1.144917494144692051E-14 ) ) ;
#19119 = CIRCLE ( 'NONE', #11876, 2.066999999999997062 ) ;
#19118 = DIRECTION ( 'NONE',  ( -1.000000000000000000, 0.000000000000000000, 0.000000000000000000 ) ) ;
#19120 = EDGE_LOOP ( 'NONE', ( #18241, #504, #19494, #5072 ) ) ;
#19121 = SHAPE_DEFINITION_REPRESENTATION ( #19712, #20540 ) ;
#19122 = EDGE_CURVE ( 'NONE', #4506, #14346, #13712, .T. ) ;
#19123 = AXIS2_PLACEMENT_3D ( 'NONE', #16659, #2306, #20471 ) ;
#19124 = ORIENTED_EDGE ( 'NONE', *, *, #16627, .T. ) ;
#19125 = AXIS2_PLACEMENT_3D ( 'NONE', #8191, #15421, #10106 ) ;
#19126 = CARTESIAN_POINT ( 'NONE',  ( -20.00000000000000000, -20.00000000000000000, -4.999999999995470290 ) ) ;
#19127 = DIRECTION ( 'NONE',  ( 0.005235963827108352890, -0.9999862922474493931, -5.936218956694023463E-19 ) ) ;
#19128 = ORIENTED_EDGE ( 'NONE', *, *, #17411, .T. ) ;
#19129 = APPROVAL ( #6783, 'UNSPECIFIED' ) ;
#19130 = CYLINDRICAL_SURFACE ( 'NONE', #3718, 3.499999999999998224 ) ;
#19131 = CC_DESIGN_DATE_AND_TIME_ASSIGNMENT ( #4751, #14123, ( #12572 ) ) ;
#19132 = CARTESIAN_POINT ( 'NONE',  ( -57.16110402867079898, 11.90787760832819941, 3.218044905330409686E-15 ) ) ;
#19133 = CARTESIAN_POINT ( 'NONE',  ( 36.38807987576970504, 8.430468791574050158, 29.25000000000000000 ) ) ;
#19134 = VERTEX_POINT ( 'NONE', #17993 ) ;
#19135 = ORIENTED_EDGE ( 'NONE', *, *, #11833, .F. ) ;
#19136 = CARTESIAN_POINT ( 'NONE',  ( 0.000000000000000000, -17.30000000000000071, -2.500000000000000000 ) ) ;
#19137 = ORIENTED_EDGE ( 'NONE', *, *, #21862, .F. ) ;
#19138 = EDGE_CURVE ( 'NONE', #8752, #11840, #22482, .T. ) ;
#19139 = EDGE_CURVE ( 'NONE', #2399, #17258, #2398, .T. ) ;
#19140 = PERSON_AND_ORGANIZATION ( #11966, #8758 ) ;
#19141 = ORIENTED_EDGE ( 'NONE', *, *, #22024, .F. ) ;
#19142 = EDGE_LOOP ( 'NONE', ( #18700, #9113, #7155, #13945 ) ) ;
#19143 = DIRECTION ( 'NONE',  ( 0.005235963827117092427, -0.9999862922474493931, -2.636227439667000721E-16 ) ) ;
#19144 = CALENDAR_DATE ( 2026, 31, 10 ) ;
#19145 = CARTESIAN_POINT ( 'NONE',  ( 50.62112045032230156, 16.80665986293769976, 3.576075166576559901E-14 ) ) ;
#19146 = CARTESIAN_POINT ( 'NONE',  ( 28.89837840081079889, -1.998294948772289858, -13.00000000000039968 ) ) ;
#19147 = PERSON_AND_ORGANIZATION_ROLE ( 'design_owner' ) ;
#19148 = ADVANCED_FACE ( 'NONE', ( #10763 ), #20978, .T. ) ;
#19149 = ORIENTED_EDGE ( 'NONE', *, *, #22822, .F. ) ;
#19150 = DIRECTION ( 'NONE',  ( -0.9997648975362233292, -0.02168293463497958373, 0.000000000000000000 ) ) ;
#19151 = CARTESIAN_POINT ( 'NONE',  ( 58.49563186522070168, 17.70675969991889787, 13.00000000000000000 ) ) ;
#19152 = ORIENTED_EDGE ( 'NONE', *, *, #13762, .F. ) ;
#19153 = DIRECTION ( 'NONE',  ( 2.269747459788999852E-13, 2.220446049250325308E-15, 1.000000000000000000 ) ) ;
#19154 = DIRECTION ( 'NONE',  ( -1.000000000000000000, 1.982541115402065307E-15, 0.000000000000000000 ) ) ;
#19155 = CARTESIAN_POINT ( 'NONE',  ( -62.82872441665799101, -8.329083101359751495, -5.528360538656857483E-15 ) ) ;
#19156 = EDGE_LOOP ( 'NONE', ( #17303, #11591, #12677, #18184 ) ) ;
#19157 = FACE_OUTER_BOUND ( 'NONE', #10140, .T. ) ;
#19158 = APPLICATION_CONTEXT ( 'configuration controlled 3d designs of mechanical parts and assemblies' ) ;
#19159 = EDGE_CURVE ( 'NONE', #21418, #6041, #7415, .T. ) ;
#19160 = PERSON_AND_ORGANIZATION ( #11966, #8758 ) ;
#19162 = EDGE_CURVE ( 'NONE', #227, #18542, #23, .T. ) ;
#19161 = VERTEX_POINT ( 'NONE', #10877 ) ;
#19163 = ORIENTED_EDGE ( 'NONE', *, *, #14756, .T. ) ;
#19164 = DIRECTION ( 'NONE',  ( -2.573454422195745135E-14, 0.000000000000000000, -1.000000000000000000 ) ) ;
#19165 = CARTESIAN_POINT ( 'NONE',  ( 36.57467860885130051, 21.71590586959130320, -11.00000000000049916 ) ) ;
#19166 = EDGE_LOOP ( 'NONE', ( #15896, #19375 ) ) ;
#19167 = CALENDAR_DATE ( 2026, 31, 10 ) ;
#19168 = DIRECTION ( 'NONE',  ( -0.005235963827108361564, 0.9999862922474493931, 3.469446951953616307E-19 ) ) ;
#19169 = CARTESIAN_POINT ( 'NONE',  ( 39.27359436029429673, 22.26288585089429972, 13.00000000000000000 ) ) ;
#19170 = CARTESIAN_POINT ( 'NONE',  ( 44.14957474989945041, 24.19027144806515039, -20.00000000000029843 ) ) ;
#19171 =( BOUNDED_CURVE ( )  B_SPLINE_CURVE ( 2, ( #19384, #3111, #8587 ),
 .UNSPECIFIED., .F., .F. ) 
 B_SPLINE_CURVE_WITH_KNOTS ( ( 3, 3 ),
 ( 0.2928548593876180162, 0.5857097187752360323 ),
 .UNSPECIFIED. ) 
 CURVE ( )  GEOMETRIC_REPRESENTATION_ITEM ( )  RATIONAL_B_SPLINE_CURVE ( ( 1.000000000000000000, 1.037954849302049842, 1.000000000000000000 ) ) 
 REPRESENTATION_ITEM ( '' )  );
#19172 =( LENGTH_UNIT ( ) NAMED_UNIT ( * ) SI_UNIT ( .MILLI., .METRE. ) );
#19173 = DIRECTION ( 'NONE',  ( 0.9730401042858035643, -0.2306359803922028717, -5.959266323858667582E-17 ) ) ;
#19174 = DATE_AND_TIME ( #17273, #1552 ) ;
#19175 = CARTESIAN_POINT ( 'NONE',  ( 37.34886511858087488, 8.673867739723879922, 8.976164948525100939 ) ) ;
#19176 = FACE_OUTER_BOUND ( 'NONE', #22117, .T. ) ;
#19177 = CC_DESIGN_PERSON_AND_ORGANIZATION_ASSIGNMENT ( #10831, #12601, ( #1591 ) ) ;
#19178 = CYLINDRICAL_SURFACE ( 'NONE', #614, 3.000000000000001332 ) ;
#19179 = DIRECTION ( 'NONE',  ( -6.662160722082822564E-09, 1.000000000000000000, -2.523234146875356491E-15 ) ) ;
#19180 = CARTESIAN_POINT ( 'NONE',  ( 37.46113131852679601, -4.027891576221570347, 20.00000000000000000 ) ) ;
#19181 = DIRECTION ( 'NONE',  ( -1.187319687680494078E-16, -2.805478249478340539E-20, -1.000000000000000000 ) ) ;
#19182 = VERTEX_POINT ( 'NONE', #18341 ) ;
#19183 = EDGE_LOOP ( 'NONE', ( #2163, #17675, #14093, #14938, #5729, #21008, #9158, #1792, #5353, #22199, #4132 ) ) ;
#19184 = LINE ( 'NONE', #22847, #13370 ) ;
#19185 = DIRECTION ( 'NONE',  ( -0.2306359803922077290, -0.9730401042858024541, 0.000000000000000000 ) ) ;
#19186 = EDGE_LOOP ( 'NONE', ( #12464, #19366, #22141, #8509 ) ) ;
#19187 = FACE_BOUND ( 'NONE', #23338, .T. ) ;
#19188 = ORIENTED_EDGE ( 'NONE', *, *, #9674, .T. ) ;
#19189 = CARTESIAN_POINT ( 'NONE',  ( 1.836479826415680084E-19, -7.772252928343919938E-16, -8.889558542813568797E-14 ) ) ;
#19190 = DATE_AND_TIME ( #11969, #18320 ) ;
#19191 = LINE ( 'NONE', #6611, #1781 ) ;
#19192 = EDGE_CURVE ( 'NONE', #16383, #19524, #17863, .T. ) ;
#19193 = DATE_AND_TIME ( #22861, #22817 ) ;
#19194 = FACE_OUTER_BOUND ( 'NONE', #10958, .T. ) ;
#19195 = PLANE ( 'NONE',  #2206 ) ;
#19196 = CARTESIAN_POINT ( 'NONE',  ( 0.000000000000000000, 0.000000000000000000, 0.000000000000000000 ) ) ;
#19197 = CARTESIAN_POINT ( 'NONE',  ( 4.267766952966368876, -31.09999999999999787, -20.76776695296636888 ) ) ;
#19198 = VERTEX_POINT ( 'NONE', #1699 ) ;
#19199 = CARTESIAN_POINT ( 'NONE',  ( 37.10730959030829723, 23.96304573415820016, 11.00000000000000000 ) ) ;
#19200 = AXIS2_PLACEMENT_3D ( 'NONE', #15907, #17459, #23133 ) ;
#19201 = FACE_OUTER_BOUND ( 'NONE', #12445, .T. ) ;
#19202 = ORIENTED_EDGE ( 'NONE', *, *, #20404, .F. ) ;
#19203 = LINE ( 'NONE', #15866, #13919 ) ;
#19204 = FACE_BOUND ( 'NONE', #799, .T. ) ;
#19205 = APPROVAL_ROLE ( '' ) ;
#19206 = CYLINDRICAL_SURFACE ( 'NONE', #17211, 1.250000000000000222 ) ;
#19207 = EDGE_LOOP ( 'NONE', ( #1870, #15294 ) ) ;
#19208 = ORIENTED_EDGE ( 'NONE', *, *, #20881, .T. ) ;
#19209 = PERSON_AND_ORGANIZATION ( #11966, #8758 ) ;
#19210 = FACE_OUTER_BOUND ( 'NONE', #10129, .T. ) ;
#19211 = ORIENTED_EDGE ( 'NONE', *, *, #1779, .T. ) ;
#19212 = CIRCLE ( 'NONE', #18079, 4.999999999999996447 ) ;
#19213 = CARTESIAN_POINT ( 'NONE',  ( -26.75617730459320143, 6.359992804688680224, -2.500000000000090150 ) ) ;
#19214 = DATE_AND_TIME ( #13755, #834 ) ;
#19215 = EDGE_CURVE ( 'NONE', #4836, #54, #3903, .T. ) ;
#19216 = CALENDAR_DATE ( 2026, 31, 10 ) ;
#19217 = LINE ( 'NONE', #8296, #12723 ) ;
#19218 = CC_DESIGN_PERSON_AND_ORGANIZATION_ASSIGNMENT ( #5651, #7446, ( #12227 ) ) ;
#19219 = CARTESIAN_POINT ( 'NONE',  ( 37.56481403710107969, 24.44795204016911327, -14.00000000000048672 ) ) ;
#19220 = ORIENTED_EDGE ( 'NONE', *, *, #1040, .F. ) ;
#19221 = ADVANCED_FACE ( 'NONE', ( #11104 ), #14536, .T. ) ;
#19222 = EDGE_CURVE ( 'NONE', #8586, #467, #864, .T. ) ;
#19223 = AXIS2_PLACEMENT_3D ( 'NONE', #20505, #2691, #16831 ) ;
#19224 = AXIS2_PLACEMENT_3D ( 'NONE', #5441, #16469, #20165 ) ;
#19225 = AXIS2_PLACEMENT_3D ( 'NONE', #21760, #19981, #16411 ) ;
#19226 = ORIENTED_EDGE ( 'NONE', *, *, #7975, .T. ) ;
#19227 = CARTESIAN_POINT ( 'NONE',  ( -14.54830929662709949, 0.3367883020382420045, 6.750000000004450662 ) ) ;
#19228 = CARTESIAN_POINT ( 'NONE',  ( 34.87444594764010475, 25.38231313435120029, -13.50000000000049916 ) ) ;
#19229 = VERTEX_POINT ( 'NONE', #21773 ) ;
#19230 = DIRECTION ( 'NONE',  ( 0.2306359803922084506, 0.9730401042858022320, -5.112869192352694760E-15 ) ) ;
#19231 = CARTESIAN_POINT ( 'NONE',  ( 44.03425675970473208, 23.70375139592372449, 13.00000000000000000 ) ) ;
#19232 = DIRECTION ( 'NONE',  ( -2.982858504577314686E-17, 2.441916418604790135E-15, 1.000000000000000000 ) ) ;
#19233 = VERTEX_POINT ( 'NONE', #19991 ) ;
#19234 = VERTEX_POINT ( 'NONE', #8850 ) ;
#19235 = LINE ( 'NONE', #6660, #17451 ) ;
#19236 = EDGE_LOOP ( 'NONE', ( #22317, #3391, #6060, #20893 ) ) ;
#19237 = APPROVAL_DATE_TIME ( #2855, #17068 ) ;
#19238 = EDGE_LOOP ( 'NONE', ( #14783, #89, #17717, #12429 ) ) ;
#19239 = ORIENTED_EDGE ( 'NONE', *, *, #20683, .F. ) ;
#19240 = CYLINDRICAL_SURFACE ( 'NONE', #14895, 5.000000000000001776 ) ;
#19241 = APPROVAL_ROLE ( '' ) ;
#19242 = EDGE_CURVE ( 'NONE', #3314, #18737, #10988, .T. ) ;
#19243 = CIRCLE ( 'NONE', #23392, 2.500000000000000000 ) ;
#19244 = DIRECTION ( 'NONE',  ( 4.028143194477080210E-16, 2.054129435991050111E-15, 1.000000000000000000 ) ) ;
#19245 = AXIS2_PLACEMENT_3D ( 'NONE', #16149, #9034, #23381 ) ;
#19246 = CC_DESIGN_DATE_AND_TIME_ASSIGNMENT ( #1732, #8759, ( #10554 ) ) ;
#19247 = PRODUCT_DEFINITION ( 'UNKNOWN', '', #19768, #21088 ) ;
#19248 = AXIS2_PLACEMENT_3D ( 'NONE', #4330, #1086, #13573 ) ;
#19249 = FACE_OUTER_BOUND ( 'NONE', #1723, .T. ) ;
#19250 = ADVANCED_FACE ( 'NONE', ( #18210 ), #1926, .T. ) ;
#19251 = EDGE_CURVE ( 'NONE', #1462, #22163, #2780, .T. ) ;
#19252 = DIRECTION ( 'NONE',  ( -0.2306359803922094498, -0.9730401042858020100, 1.412237191019847142E-17 ) ) ;
#19253 = CALENDAR_DATE ( 2026, 31, 10 ) ;
#19254 = CC_DESIGN_PERSON_AND_ORGANIZATION_ASSIGNMENT ( #4496, #15410, ( #15527 ) ) ;
#19255 = ORIENTED_EDGE ( 'NONE', *, *, #740, .T. ) ;
#19256 = VECTOR ( 'NONE', #17090, 1000.000000000000000 ) ;
#19257 = DIRECTION ( 'NONE',  ( -1.000000000000000000, 2.270069654138870255E-15, -3.099353312215989243E-62 ) ) ;
#19258 = CARTESIAN_POINT ( 'NONE',  ( -22.50000000397270128, 22.95208917591822129, 6.750000000004498624 ) ) ;
#19259 = EDGE_LOOP ( 'NONE', ( #22665, #5150, #5767, #8201 ) ) ;
#19260 = CIRCLE ( 'NONE', #1414, 9.000000000000005329 ) ;
#19261 = CIRCLE ( 'NONE', #9024, 2.499999999999998668 ) ;
#19262 = DIRECTION ( 'NONE',  ( 1.187319687680494078E-16, 2.805478249478255076E-20, 1.000000000000000000 ) ) ;
#19264 = AXIS2_PLACEMENT_3D ( 'NONE', #11240, #20469, #4087 ) ;
#19263 = CARTESIAN_POINT ( 'NONE',  ( 117.1241794131700118, -12.63305097454420078, -15.90000000000000036 ) ) ;
#19265 = CARTESIAN_POINT ( 'NONE',  ( -24.50000000000000000, -30.47499999999999787, 19.00000000000000000 ) ) ;
#19266 = ORIENTED_EDGE ( 'NONE', *, *, #4139, .T. ) ;
#19267 = CARTESIAN_POINT ( 'NONE',  ( -14.54830929633980041, -2.787889851644890005, -6.749999999996740385 ) ) ;
#19268 = CALENDAR_DATE ( 2026, 31, 10 ) ;
#19269 = ORIENTED_EDGE ( 'NONE', *, *, #4469, .F. ) ;
#19270 = VERTEX_POINT ( 'NONE', #148 ) ;
#19271 = DIRECTION ( 'NONE',  ( -3.715058581704769953E-16, 5.072287515438380936E-15, 1.000000000000000000 ) ) ;
#19272 = CARTESIAN_POINT ( 'NONE',  ( 6.500000000000000000, -1.630990338096509915E-14, 2.500000000000000000 ) ) ;
#19273 = CARTESIAN_POINT ( 'NONE',  ( 29.89447396975369742, -1.047702001782899961, 11.00000000000019895 ) ) ;
#19274 = CIRCLE ( 'NONE', #9405, 2.500000000000000000 ) ;
#19275 = APPROVAL_DATE_TIME ( #21162, #18376 ) ;
#19276 = DIRECTION ( 'NONE',  ( -2.269700743865584947E-13, -2.220446049247695246E-15, -1.000000000000000000 ) ) ;
#19277 = EDGE_CURVE ( 'NONE', #16326, #8980, #19458, .T. ) ;
#19278 = DIRECTION ( 'NONE',  ( -1.751019220569994795E-16, -2.300154215587015208E-15, -1.000000000000000000 ) ) ;
#19279 = AXIS2_PLACEMENT_3D ( 'NONE', #22777, #6289, #15420 ) ;
#19280 = DIRECTION ( 'NONE',  ( -1.000000000000000000, 0.000000000000000000, 0.000000000000000000 ) ) ;
#19281 = CONICAL_SURFACE ( 'NONE', #6000, 0.8660254037844395958, 1.047197551196598297 ) ;
#19282 = ADVANCED_FACE ( 'NONE', ( #14647 ), #10767, .T. ) ;
#19283 = CYLINDRICAL_SURFACE ( 'NONE', #14721, 2.500000000000000000 ) ;
#19284 = PERSON_AND_ORGANIZATION ( #11966, #8758 ) ;
#19285 = EDGE_CURVE ( 'NONE', #4850, #13082, #20104, .T. ) ;
#19286 = CARTESIAN_POINT ( 'NONE',  ( -26.00000000397439948, 22.95208919201850151, -6.749999999994200195 ) ) ;
#19287 = DIRECTION ( 'NONE',  ( 0.5249589903860194529, -0.8511275218278935295, 5.444325428271645316E-17 ) ) ;
#19288 = DIRECTION ( 'NONE',  ( 0.9999862922474492821, 0.005235963827108391054, 0.000000000000000000 ) ) ;
#19289 = DIRECTION ( 'NONE',  ( 0.9730401042858024541, -0.2306359803922080898, -5.959266323859062013E-17 ) ) ;
#19290 = DIRECTION ( 'NONE',  ( 8.911056267098788616E-18, 1.998401444326210262E-15, 1.000000000000000000 ) ) ;
#19291 = ORIENTED_EDGE ( 'NONE', *, *, #3592, .T. ) ;
#19292 = CARTESIAN_POINT ( 'NONE',  ( -62.73971250800079957, -25.32895006819559924, -5.538452170245418869E-15 ) ) ;
#19293 = VERTEX_POINT ( 'NONE', #16082 ) ;
#19294 = EDGE_LOOP ( 'NONE', ( #6768, #8108, #8406, #8812 ) ) ;
#19295 = DIRECTION ( 'NONE',  ( -3.099353312215989243E-62, 1.001855809244433740E-92, 1.000000000000000000 ) ) ;
#19296 = CIRCLE ( 'NONE', #20048, 4.250000000000001776 ) ;
#19297 = DIRECTION ( 'NONE',  ( 0.9730401042858036753, -0.2306359803922031493, 6.356122819266963936E-16 ) ) ;
#19298 = ORIENTED_EDGE ( 'NONE', *, *, #12170, .F. ) ;
#19299 = DIRECTION ( 'NONE',  ( 1.000000000000000000, 7.664170260637140280E-16, 0.000000000000000000 ) ) ;
#19300 = PERSON ( 'NAUO-PER7', 'UNSPECIFIED', 'UNSPECIFIED', ('UNSPECIFIED'), ('UNSPECIFIED'), ('UNSPECIFIED') ) ;
#19301 = VERTEX_POINT ( 'NONE', #23312 ) ;
#19302 = DIRECTION ( 'NONE',  ( -1.187319687680494078E-16, -2.805478249478340539E-20, -1.000000000000000000 ) ) ;
#19303 = SHAPE_REPRESENTATION ( 'Latching', ( #15386, #17301, #7068, #5537, #13126, #2887, #16146, #21220, #2649, #15170, #9110, #22363, #20080, #17048, #18595, #6831, #4544, #9486 ), #12166 ) ;
#19304 = CALENDAR_DATE ( 2026, 31, 10 ) ;
#19305 = DIRECTION ( 'NONE',  ( 0.1153179901961009640, 0.4865200521429018377, -0.8660254037844385966 ) ) ;
#19306 = ADVANCED_FACE ( 'NONE', ( #7071 ), #14992, .T. ) ;
#19307 = DATE_AND_TIME ( #17412, #432 ) ;
#19308 = DIRECTION ( 'NONE',  ( -0.9730401042858036753, 0.2306359803922023999, -1.110223024625155524E-17 ) ) ;
#19309 = ADVANCED_FACE ( 'NONE', ( #7874 ), #9548, .F. ) ;
#19310 = FACE_OUTER_BOUND ( 'NONE', #22788, .T. ) ;
#19311 = DIRECTION ( 'NONE',  ( -6.662111140531837817E-09, 1.000000000000000000, -2.081668171172169697E-15 ) ) ;
#19312 = ORIENTED_EDGE ( 'NONE', *, *, #5454, .F. ) ;
#19313 = DIRECTION ( 'NONE',  ( -1.469367938527859874E-40, 1.000000000000000000, -9.249283497051789705E-11 ) ) ;
#19314 = CARTESIAN_POINT ( 'NONE',  ( 0.000000000000000000, -3.886126572655959799E-16, -2.500000000000000000 ) ) ;
#19315 = VERTEX_POINT ( 'NONE', #4323 ) ;
#19316 = CARTESIAN_POINT ( 'NONE',  ( 33.55185054466894456, 10.12066834538196147, -9.000012392934834793 ) ) ;
#19317 = VECTOR ( 'NONE', #20483, 1000.000000000000000 ) ;
#19318 = CARTESIAN_POINT ( 'NONE',  ( 45.98502771169970060, -8.172548290408343519, 13.00000000000000000 ) ) ;
#19319 = APPROVAL_DATE_TIME ( #14089, #12270 ) ;
#19320 = DIRECTION ( 'NONE',  ( -0.9730401042858024541, 0.2306359803922080898, 5.959266323863162857E-17 ) ) ;
#19321 = ORIENTED_EDGE ( 'NONE', *, *, #6057, .T. ) ;
#19322 = ORIENTED_EDGE ( 'NONE', *, *, #18777, .F. ) ;
#19323 = DATE_AND_TIME ( #13511, #20547 ) ;
#19324 = CARTESIAN_POINT ( 'NONE',  ( 37.27955344062029752, 9.375336445360519022, -28.47000000000049980 ) ) ;
#19325 = EDGE_LOOP ( 'NONE', ( #20481, #15726, #5601 ) ) ;
#19326 = CARTESIAN_POINT ( 'NONE',  ( -20.00000000000000000, -20.00000000000000000, 2.500000000000000000 ) ) ;
#19327 = APPLICATION_CONTEXT ( 'configuration controlled 3d designs of mechanical parts and assemblies' ) ;
#19328 = PERSON_AND_ORGANIZATION_ROLE ( 'classification_officer' ) ;
#19329 = PRODUCT ( 'Pin 3', 'Pin 3', '', ( #20455 ) ) ;
#19330 = COORDINATED_UNIVERSAL_TIME_OFFSET ( 0, 0, .AHEAD. ) ;
#19331 = DIRECTION ( 'NONE',  ( 3.211814849206744928E-17, -2.442368445299930211E-15, -1.000000000000000000 ) ) ;
#19332 = ORGANIZATION ( 'NAUO-ORG11', 'UNSPECIFIED', 'UNSPECIFIED' ) ;
#19333 = CIRCLE ( 'NONE', #15531, 0.09999999999999999167 ) ;
#19334 = DIRECTION ( 'NONE',  ( -2.269747459788994803E-13, -2.220446049250305192E-15, -1.000000000000000000 ) ) ;
#19335 = ORIENTED_EDGE ( 'NONE', *, *, #22048, .F. ) ;
#19336 = EDGE_LOOP ( 'NONE', ( #11588, #167 ) ) ;
#19337 = FACE_OUTER_BOUND ( 'NONE', #7961, .T. ) ;
#19338 = CARTESIAN_POINT ( 'NONE',  ( 6.500000000000000000, -1.630990338096509915E-14, 5.000000000000000000 ) ) ;
#19340 = VERTEX_POINT ( 'NONE', #16642 ) ;
#19339 = ADVANCED_FACE ( 'NONE', ( #9678 ), #7998, .F. ) ;
#19341 = ADVANCED_FACE ( 'NONE', ( #18574 ), #13110, .F. ) ;
#19342 = DIRECTION ( 'NONE',  ( -6.123230199561449365E-17, -4.868008300101910084E-15, -1.000000000000000000 ) ) ;
#19343 = LINE ( 'NONE', #8776, #19507 ) ;
#19344 = CARTESIAN_POINT ( 'NONE',  ( -19.49999999982360066, -0.1021026942259779940, -3.750000000000000000 ) ) ;
#19345 = AXIS2_PLACEMENT_3D ( 'NONE', #12319, #16088, #14295 ) ;
#19346 = ORIENTED_EDGE ( 'NONE', *, *, #16374, .F. ) ;
#19347 =( GEOMETRIC_REPRESENTATION_CONTEXT ( 3 ) GLOBAL_UNCERTAINTY_ASSIGNED_CONTEXT ( ( #17991 ) ) GLOBAL_UNIT_ASSIGNED_CONTEXT ( ( #3210, #17711, #17942 ) ) REPRESENTATION_CONTEXT ( 'NONE', 'WORKASPACE' ) );
#19348 = ORIENTED_EDGE ( 'NONE', *, *, #23080, .T. ) ;
#19350 = AXIS2_PLACEMENT_3D ( 'NONE', #16501, #14152, #23282 ) ;
#19349 = DIRECTION ( 'NONE',  ( 0.000000000000000000, -1.000000000000000000, 2.081668171172168119E-15 ) ) ;
#19351 = EDGE_LOOP ( 'NONE', ( #13618, #12118 ) ) ;
#19352 = APPLICATION_PROTOCOL_DEFINITION ( 'international standard', 'config_control_design', 1994, #6251 ) ;
#19353 = ORIENTED_EDGE ( 'NONE', *, *, #13173, .F. ) ;
#19354 = ORIENTED_EDGE ( 'NONE', *, *, #20053, .F. ) ;
#19355 = CARTESIAN_POINT ( 'NONE',  ( 62.70840910389689782, 3.348031886875269869, 1.061114750357439988E-14 ) ) ;
#19356 = COORDINATED_UNIVERSAL_TIME_OFFSET ( 0, 0, .AHEAD. ) ;
#19357 = VECTOR ( 'NONE', #2045, 1000.000000000000000 ) ;
#19358 = ADVANCED_FACE ( 'NONE', ( #16891 ), #2643, .T. ) ;
#19359 = EDGE_CURVE ( 'NONE', #12704, #14320, #623, .T. ) ;
#19360 = FACE_OUTER_BOUND ( 'NONE', #2106, .T. ) ;
#19361 = AXIS2_PLACEMENT_3D ( 'NONE', #9404, #5843, #13091 ) ;
#19362 = CC_DESIGN_APPROVAL ( #17382, ( #7614 ) ) ;
#19363 = AXIS2_PLACEMENT_3D ( 'NONE', #15066, #15625, #3031 ) ;
#19364 = CARTESIAN_POINT ( 'NONE',  ( 28.67817383939640052, -0.7594070262926440051, 15.00000000000000000 ) ) ;
#19365 = APPROVAL_STATUS ( 'not_yet_approved' ) ;
#19366 = ORIENTED_EDGE ( 'NONE', *, *, #19771, .T. ) ;
#19367 = CARTESIAN_POINT ( 'NONE',  ( 31.11077410011089839, -1.335996977273150144, 11.00000000000019895 ) ) ;
#19368 = FACE_OUTER_BOUND ( 'NONE', #17096, .T. ) ;
#19369 = AXIS2_PLACEMENT_3D ( 'NONE', #19716, #10015, #4003 ) ;
#19370 = EDGE_LOOP ( 'NONE', ( #22441, #19987, #11808, #16615 ) ) ;
#19371 = ADVANCED_FACE ( 'NONE', ( #17130, #22342 ), #6219, .T. ) ;
#19372 = DIRECTION ( 'NONE',  ( -0.4999931461237248076, -0.002617981913554119633, -0.8660254037844385966 ) ) ;
#19373 = DIRECTION ( 'NONE',  ( -1.187319687680499994E-16, -2.805478249478705262E-20, -1.000000000000000000 ) ) ;
#19374 = PLANE ( 'NONE',  #21330 ) ;
#19375 = ORIENTED_EDGE ( 'NONE', *, *, #19072, .T. ) ;
#19376 = CYLINDRICAL_SURFACE ( 'NONE', #448, 2.499999999999998668 ) ;
#19377 = CLOSED_SHELL ( 'NONE', ( #15150, #3140, #8339, #17246, #12963, #14941 ) ) ;
#19378 = CC_DESIGN_PERSON_AND_ORGANIZATION_ASSIGNMENT ( #3907, #12709, ( #11759 ) ) ;
#19379 = PERSON_AND_ORGANIZATION ( #11966, #8758 ) ;
#19380 = APPROVAL_PERSON_ORGANIZATION ( #5107, #19543, #2963 ) ;
#19381 = EDGE_LOOP ( 'NONE', ( #10757, #13765, #23047, #12839 ) ) ;
#19382 = PRODUCT_DEFINITION ( 'UNKNOWN', '', #11856, #3038 ) ;
#19383 = ORIENTED_EDGE ( 'NONE', *, *, #16626, .F. ) ;
#19384 = CARTESIAN_POINT ( 'NONE',  ( -67.06978017061331343, -25.35162245663349978, 2.500000000000000000 ) ) ;
#19385 = CARTESIAN_POINT ( 'NONE',  ( -60.04781580374580585, 11.89276268270289982, 5.000000000000000000 ) ) ;
#19386 = APPROVAL_PERSON_ORGANIZATION ( #15082, #21860, #22439 ) ;
#19387 = CARTESIAN_POINT ( 'NONE',  ( 50.76434296088209663, 17.41090750189739822, 3.560102062092729998E-14 ) ) ;
#19388 = PERSON_AND_ORGANIZATION ( #11966, #8758 ) ;
#19389 = EDGE_CURVE ( 'NONE', #3393, #2620, #20694, .T. ) ;
#19390 = LINE ( 'NONE', #17733, #21372 ) ;
#19391 = EDGE_CURVE ( 'NONE', #20204, #13560, #6324, .T. ) ;
#19392 = VECTOR ( 'NONE', #22279, 1000.000000000000227 ) ;
#19393 = LINE ( 'NONE', #5247, #8750 ) ;
#19394 = DIRECTION ( 'NONE',  ( -1.000000000000000000, 0.000000000000000000, -3.525869238601989755E-16 ) ) ;
#19395 = AXIS2_PLACEMENT_3D ( 'NONE', #8742, #21200, #15978 ) ;
#19396 = CARTESIAN_POINT ( 'NONE',  ( -62.74088165156670271, -25.10566213532069924, -5.538319619822460249E-15 ) ) ;
#19397 = DATE_AND_TIME ( #6703, #17123 ) ;
#19398 = PRODUCT_DEFINITION_FORMATION_WITH_SPECIFIED_SOURCE ( 'ANY', '', #7215, .NOT_KNOWN. ) ;
#19399 = CC_DESIGN_APPROVAL ( #3641, ( #6840 ) ) ;
#19400 = CARTESIAN_POINT ( 'NONE',  ( 35.79117365064221445, 7.712783139516915298, 8.783920975641617446 ) ) ;
#19401 = CARTESIAN_POINT ( 'NONE',  ( -60.02994014102380049, 8.478793778983318319, 5.000000000000000000 ) ) ;
#19402 = CYLINDRICAL_SURFACE ( 'NONE', #22227, 2.066999999999999726 ) ;
#19403 = EDGE_CURVE ( 'NONE', #21838, #4561, #16040, .T. ) ;
#19404 = CYLINDRICAL_SURFACE ( 'NONE', #7860, 5.000000000000000888 ) ;
#19405 = CARTESIAN_POINT ( 'NONE',  ( 31.49419854219519976, 9.774809681453278998, -23.00000000000000000 ) ) ;
#19406 = ORIENTED_EDGE ( 'NONE', *, *, #16363, .T. ) ;
#19407 = PERSON_AND_ORGANIZATION_ROLE ( 'design_owner' ) ;
#19408 = LINE ( 'NONE', #23186, #12639 ) ;
#19409 = UNCERTAINTY_MEASURE_WITH_UNIT (LENGTH_MEASURE( 1.000000000000000082E-05 ), #12292, 'distance_accuracy_value', 'NONE');
#19410 = ORIENTED_EDGE ( 'NONE', *, *, #10235, .T. ) ;
#19411 = DIRECTION ( 'NONE',  ( 0.000000000000000000, -1.000000000000000000, 0.000000000000000000 ) ) ;
#19412 = CARTESIAN_POINT ( 'NONE',  ( -26.75688440168130100, 6.359989102302520791, 2.500292893218799772 ) ) ;
#19413 = ORIENTED_EDGE ( 'NONE', *, *, #19537, .F. ) ;
#19414 = EDGE_CURVE ( 'NONE', #11308, #11527, #8854, .T. ) ;
#19415 = CARTESIAN_POINT ( 'NONE',  ( 41.24356139695900225, 11.92996613406550033, -18.89999999999999858 ) ) ;
#19416 = EDGE_CURVE ( 'NONE', #23152, #3517, #505, .T. ) ;
#19417 = ORIENTED_EDGE ( 'NONE', *, *, #7481, .F. ) ;
#19418 = APPROVAL_PERSON_ORGANIZATION ( #18924, #2542, #15113 ) ;
#19419 = DIRECTION ( 'NONE',  ( 0.000000000000000000, 0.000000000000000000, 1.000000000000000000 ) ) ;
#19420 = APPROVAL_ROLE ( '' ) ;
#19421 = CARTESIAN_POINT ( 'NONE',  ( -26.99999999999959854, -31.09999999999999787, 21.50000000000000000 ) ) ;
#19422 = CALENDAR_DATE ( 2026, 31, 10 ) ;
#19423 = ORGANIZATION ( 'NAUO-ORG28', 'UNSPECIFIED', 'UNSPECIFIED' ) ;
#19424 = DIRECTION ( 'NONE',  ( 3.210834492181045054E-17, -2.441916418604790135E-15, -1.000000000000000000 ) ) ;
#19425 = PLANE ( 'NONE',  #6759 ) ;
#19426 = DIRECTION ( 'NONE',  ( 3.099353312215988811E-62, -1.534091707905539548E-92, -1.000000000000000000 ) ) ;
#19427 = ORIENTED_EDGE ( 'NONE', *, *, #23469, .T. ) ;
#19428 = FACE_OUTER_BOUND ( 'NONE', #19156, .T. ) ;
#19429 = EDGE_CURVE ( 'NONE', #22544, #22391, #11464, .T. ) ;
#19430 = LOCAL_TIME ( 14, 11, 27.00000000000000000, #14128 ) ;
#19431 = LINE ( 'NONE', #4823, #6889 ) ;
#19432 = ORIENTED_EDGE ( 'NONE', *, *, #22486, .T. ) ;
#19433 = DIRECTION ( 'NONE',  ( 0.9730401042858034533, -0.2306359803922026774, 1.869849304631839730E-15 ) ) ;
#19434 = VECTOR ( 'NONE', #15702, 1000.000000000000114 ) ;
#19435 = PLANE ( 'NONE',  #21639 ) ;
#19436 = VECTOR ( 'NONE', #22960, 1000.000000000000000 ) ;
#19437 = ORIENTED_EDGE ( 'NONE', *, *, #14740, .T. ) ;
#19438 = PERSON_AND_ORGANIZATION_ROLE ( 'classification_officer' ) ;
#19439 = AXIS2_PLACEMENT_3D ( 'NONE', #11873, #15054, #4724 ) ;
#19440 = DIRECTION ( 'NONE',  ( 0.000000000000000000, 0.000000000000000000, 1.000000000000000000 ) ) ;
#19441 =( BOUNDED_CURVE ( )  B_SPLINE_CURVE ( 2, ( #4897, #15820, #22816 ),
 .UNSPECIFIED., .F., .F. ) 
 B_SPLINE_CURVE_WITH_KNOTS ( ( 3, 3 ),
 ( 0.000000000000000000, 0.5842180690389578990 ),
 .UNSPECIFIED. ) 
 CURVE ( )  GEOMETRIC_REPRESENTATION_ITEM ( )  RATIONAL_B_SPLINE_CURVE ( ( 1.000000000000000000, 1.154700538379249908, 1.000000000000000000 ) ) 
 REPRESENTATION_ITEM ( '' )  );
#19442 = ORIENTED_EDGE ( 'NONE', *, *, #19814, .T. ) ;
#19443 = ORGANIZATION ( 'NAUO-ORG34', 'UNSPECIFIED', 'UNSPECIFIED' ) ;
#19444 = EDGE_LOOP ( 'NONE', ( #15020, #11781 ) ) ;
#19445 = EDGE_CURVE ( 'NONE', #12377, #2029, #17954, .T. ) ;
#19446 = PERSON_AND_ORGANIZATION ( #11966, #8758 ) ;
#19447 = VECTOR ( 'NONE', #7629, 1000.000000000000227 ) ;
#19448 = CYLINDRICAL_SURFACE ( 'NONE', #6921, 3.499999999999998668 ) ;
#19449 = ORIENTED_EDGE ( 'NONE', *, *, #19072, .F. ) ;
#19450 = ADVANCED_FACE ( 'NONE', ( #14879 ), #4072, .T. ) ;
#19451 = DIRECTION ( 'NONE',  ( 0.9730401042858035643, -0.2306359803922028717, -5.959266323858677443E-17 ) ) ;
#19452 = CIRCLE ( 'NONE', #10758, 4.100000000000000533 ) ;
#19453 = APPROVAL_ROLE ( '' ) ;
#19454 = CC_DESIGN_APPROVAL ( #10120, ( #7318 ) ) ;
#19455 = APPROVAL_DATE_TIME ( #3294, #14439 ) ;
#19456 = DIRECTION ( 'NONE',  ( -0.2306359803922090057, -0.9730401042858021210, 4.744007713284281930E-15 ) ) ;
#19457 = VECTOR ( 'NONE', #15894, 1000.000000000000000 ) ;
#19458 = CIRCLE ( 'NONE', #4680, 15.25000000000000000 ) ;
#19459 = VECTOR ( 'NONE', #3986, 999.9999999999998863 ) ;
#19460 = CYLINDRICAL_SURFACE ( 'NONE', #13052, 2.499999999999998668 ) ;
#19461 = ORIENTED_EDGE ( 'NONE', *, *, #21558, .T. ) ;
#19462 = VERTEX_POINT ( 'NONE', #2527 ) ;
#19463 = VECTOR ( 'NONE', #21781, 999.9999999999998863 ) ;
#19464 = DIRECTION ( 'NONE',  ( 0.9730401042858024541, -0.2306359803922080898, -5.959266323858942451E-17 ) ) ;
#19465 = DIRECTION ( 'NONE',  ( -0.2306359803922076457, -0.9730401042858025651, 0.000000000000000000 ) ) ;
#19466 = ORIENTED_EDGE ( 'NONE', *, *, #17176, .T. ) ;
#19467 = VECTOR ( 'NONE', #100, 1000.000000000000114 ) ;
#19468 = CC_DESIGN_PERSON_AND_ORGANIZATION_ASSIGNMENT ( #9, #3702, ( #6840 ) ) ;
#19469 = CC_DESIGN_SECURITY_CLASSIFICATION ( #15292, ( #19087 ) ) ;
#19470 = CARTESIAN_POINT ( 'NONE',  ( 28.65327419723657343, 2.170628644843063615, -6.523238081173185874E-16 ) ) ;
#19471 = CARTESIAN_POINT ( 'NONE',  ( -20.00000000397360012, 22.95208919256889857, -2.500000000000039968 ) ) ;
#19472 = EDGE_LOOP ( 'NONE', ( #20095, #18603, #7987, #11910, #14087 ) ) ;
#19473 = VERTEX_POINT ( 'NONE', #9787 ) ;
#19474 = CARTESIAN_POINT ( 'NONE',  ( -20.00000000000000000, -20.00000000000000000, -5.499999999995469402 ) ) ;
#19475 = AXIS2_PLACEMENT_3D ( 'NONE', #2443, #2311, #13806 ) ;
#19476 = ORIENTED_EDGE ( 'NONE', *, *, #14641, .F. ) ;
#19477 = AXIS2_PLACEMENT_3D ( 'NONE', #23050, #6803, #12282 ) ;
#19478 = APPLICATION_PROTOCOL_DEFINITION ( 'international standard', 'config_control_design', 1994, #10667 ) ;
#19479 = EDGE_LOOP ( 'NONE', ( #23379, #9906, #5916, #71, #19208, #9973 ) ) ;
#19480 = VECTOR ( 'NONE', #8476, 1000.000000000000114 ) ;
#19481 = ORIENTED_EDGE ( 'NONE', *, *, #16413, .T. ) ;
#19482 = DIRECTION ( 'NONE',  ( -0.9730401042858035643, 0.2306359803922028717, 6.126766849694256332E-17 ) ) ;
#19483 = PERSON_AND_ORGANIZATION ( #11966, #8758 ) ;
#19484 = DIRECTION ( 'NONE',  ( -1.000000000000000000, 0.000000000000000000, 0.000000000000000000 ) ) ;
#19485 = CIRCLE ( 'NONE', #2748, 7.999999999999998224 ) ;
#19486 = EDGE_CURVE ( 'NONE', #10370, #20679, #19504, .T. ) ;
#19487 = VECTOR ( 'NONE', #19924, 1000.000000000000000 ) ;
#19488 = CARTESIAN_POINT ( 'NONE',  ( 52.26033179423370001, -7.535689554643850485, 13.00000000000019895 ) ) ;
#19489 = TOROIDAL_SURFACE ( 'NONE', #14573, 5.000000000000000000, 3.000000000000000000 ) ;
#19490 = DATE_TIME_ROLE ( 'classification_date' ) ;
#19491 = ORIENTED_EDGE ( 'NONE', *, *, #4870, .T. ) ;
#19492 = DIRECTION ( 'NONE',  ( -0.9730401042858022320, 0.2306359803922080343, 5.959266323858941219E-17 ) ) ;
#19493 = CARTESIAN_POINT ( 'NONE',  ( 113.4570673249340018, -28.10438863268850085, 2.700000000000049916 ) ) ;
#19494 = ORIENTED_EDGE ( 'NONE', *, *, #10914, .T. ) ;
#19495 = CARTESIAN_POINT ( 'NONE',  ( 117.1011158151309957, -12.73035498497280038, 19.59999999999999787 ) ) ;
#19496 = CYLINDRICAL_SURFACE ( 'NONE', #1655, 2.500000000000000444 ) ;
#19497 = DIRECTION ( 'NONE',  ( -0.7071067811865475727, 1.387778780781445281E-15, 0.7071067811865475727 ) ) ;
#19498 = ORIENTED_EDGE ( 'NONE', *, *, #1944, .F. ) ;
#19499 = LINE ( 'NONE', #11935, #8070 ) ;
#19500 = DATE_AND_TIME ( #17479, #3066 ) ;
#19501 = CIRCLE ( 'NONE', #9265, 2.009239999999998805 ) ;
#19502 = ORIENTED_EDGE ( 'NONE', *, *, #18292, .T. ) ;
#19503 = ORIENTED_EDGE ( 'NONE', *, *, #6190, .T. ) ;
#19504 = LINE ( 'NONE', #12156, #8482 ) ;
#19505 = FACE_OUTER_BOUND ( 'NONE', #1034, .T. ) ;
#19506 = LINE ( 'NONE', #12502, #11847 ) ;
#19507 = VECTOR ( 'NONE', #15785, 1000.000000000000000 ) ;
#19508 = SECURITY_CLASSIFICATION_LEVEL ( 'unclassified' ) ;
#19509 = PLANE ( 'NONE',  #8858 ) ;
#19510 = DIRECTION ( 'NONE',  ( 0.8511275218278948618, 0.5249589903860170104, -5.212440122911309516E-17 ) ) ;
#19511 = EDGE_CURVE ( 'NONE', #19822, #5968, #967, .T. ) ;
#19512 = DIRECTION ( 'NONE',  ( 0.000000000000000000, 0.000000000000000000, 1.000000000000000000 ) ) ;
#19513 = CC_DESIGN_DATE_AND_TIME_ASSIGNMENT ( #7694, #5798, ( #22065 ) ) ;
#19514 = ORIENTED_EDGE ( 'NONE', *, *, #8270, .T. ) ;
#19515 = CARTESIAN_POINT ( 'NONE',  ( 0.000000000000000000, -17.30000000000000071, -2.500000000000000000 ) ) ;
#19516 = DATE_TIME_ROLE ( 'classification_date' ) ;
#19517 = CARTESIAN_POINT ( 'NONE',  ( 35.11747397072458199, 7.763535785894707608, 8.759424124906642461 ) ) ;
#19518 = DIRECTION ( 'NONE',  ( -0.9730401042858022320, 0.2306359803922080343, 5.959266323858941219E-17 ) ) ;
#19519 = EDGE_CURVE ( 'NONE', #18262, #9929, #15679, .T. ) ;
#19520 = EDGE_CURVE ( 'NONE', #23364, #23217, #22815, .T. ) ;
#19521 = CARTESIAN_POINT ( 'NONE',  ( 52.45828777336780036, 19.13776831658130106, -13.00000000000000000 ) ) ;
#19522 = CARTESIAN_POINT ( 'NONE',  ( -11.24263882182209962, 20.87636639668270178, -2.500000000000000000 ) ) ;
#19523 = DIRECTION ( 'NONE',  ( 1.138590270679730064E-14, 2.220446049251240387E-15, 1.000000000000000000 ) ) ;
#19524 = VERTEX_POINT ( 'NONE', #10259 ) ;
#19525 = LINE ( 'NONE', #15487, #21718 ) ;
#19526 = PRODUCT ( 'Electric Motor', 'Electric Motor', '', ( #11604 ) ) ;
#19527 = ORIENTED_EDGE ( 'NONE', *, *, #15483, .F. ) ;
#19528 = CARTESIAN_POINT ( 'NONE',  ( -60.05196788195259927, 12.68574396146170180, 5.000000000000000000 ) ) ;
#19529 = CARTESIAN_POINT ( 'NONE',  ( 35.59419854219520118, 9.774809681453278998, -26.88000000000049994 ) ) ;
#19530 = ORIENTED_EDGE ( 'NONE', *, *, #15220, .F. ) ;
#19531 = DIRECTION ( 'NONE',  ( 1.000000000000000000, -4.539762594625140272E-47, -7.773397468430785553E-78 ) ) ;
#19532 = ORIENTED_EDGE ( 'NONE', *, *, #7941, .T. ) ;
#19533 = CIRCLE ( 'NONE', #18800, 3.499999999999999556 ) ;
#19534 = DIRECTION ( 'NONE',  ( 0.7194962871189621856, 0.6944962871189651610, 2.229973200609260484E-62 ) ) ;
#19535 = APPROVAL_STATUS ( 'not_yet_approved' ) ;
#19536 = FACE_OUTER_BOUND ( 'NONE', #18776, .T. ) ;
#19537 = EDGE_CURVE ( 'NONE', #13627, #22148, #11537, .T. ) ;
#19538 = SHAPE_REPRESENTATION_RELATIONSHIP ( 'NONE' , 'NONE' ,  #11141, #6259 ) ;
#19539 = CARTESIAN_POINT ( 'NONE',  ( -28.45655959278310121, -6.649088660734180145, -0.7325259402522680263 ) ) ;
#19540 = CC_DESIGN_PERSON_AND_ORGANIZATION_ASSIGNMENT ( #18902, #22558, ( #7661 ) ) ;
#19541 = DIRECTION ( 'NONE',  ( -4.040376328279780192E-15, 1.000000000000000000, -1.816625962794309743E-30 ) ) ;
#19542 =( NAMED_UNIT ( * ) PLANE_ANGLE_UNIT ( ) SI_UNIT ( $, .RADIAN. ) );
#19543 = APPROVAL ( #8672, 'UNSPECIFIED' ) ;
#19544 = CARTESIAN_POINT ( 'NONE',  ( -69.82862846239015653, -8.365734848149525504, 7.200000000000000178 ) ) ;
#19545 = ORIENTED_EDGE ( 'NONE', *, *, #13891, .F. ) ;
#19546 = DIRECTION ( 'NONE',  ( 0.000000000000000000, 1.000000000000000000, 0.000000000000000000 ) ) ;
#19547 = EDGE_CURVE ( 'NONE', #3952, #990, #10382, .T. ) ;
#19548 = EDGE_CURVE ( 'NONE', #3201, #23008, #22500, .T. ) ;
#19549 = PERSON ( 'NAUO-PER14', 'UNSPECIFIED', 'UNSPECIFIED', ('UNSPECIFIED'), ('UNSPECIFIED'), ('UNSPECIFIED') ) ;
#19550 =( GEOMETRIC_REPRESENTATION_CONTEXT ( 3 ) GLOBAL_UNCERTAINTY_ASSIGNED_CONTEXT ( ( #1339 ) ) GLOBAL_UNIT_ASSIGNED_CONTEXT ( ( #22266, #13255, #18747 ) ) REPRESENTATION_CONTEXT ( 'NONE', 'WORKASPACE' ) );
#19551 = LINE ( 'NONE', #10656, #1930 ) ;
#19552 = PRODUCT_DEFINITION ( 'UNKNOWN', '', #21633, #10436 ) ;
#19553 = ORIENTED_EDGE ( 'NONE', *, *, #21508, .F. ) ;
#19554 = FACE_OUTER_BOUND ( 'NONE', #8420, .T. ) ;
#19555 = CARTESIAN_POINT ( 'NONE',  ( -11.34268231757140022, -0.05939068843019929683, -8.754884475926699325E-14 ) ) ;
#19556 = ORIENTED_EDGE ( 'NONE', *, *, #8180, .F. ) ;
#19557 = APPROVAL_ROLE ( '' ) ;
#19558 = FACE_OUTER_BOUND ( 'NONE', #5526, .T. ) ;
#19559 = EDGE_LOOP ( 'NONE', ( #16890, #17690, #9252, #4372 ) ) ;
#19560 = VERTEX_POINT ( 'NONE', #2767 ) ;
#19561 = PERSON_AND_ORGANIZATION ( #11966, #8758 ) ;
#19562 = DIRECTION ( 'NONE',  ( 0.9730401042858035643, -0.2306359803922028717, -5.432877459303547053E-17 ) ) ;
#19563 = ORIENTED_EDGE ( 'NONE', *, *, #10678, .T. ) ;
#19564 = DIRECTION ( 'NONE',  ( -0.9997651245102161521, -0.02167246670483386276, 0.000000000000000000 ) ) ;
#19565 = PERSON_AND_ORGANIZATION ( #11966, #8758 ) ;
#19566 = ADVANCED_FACE ( 'NONE', ( #23159 ), #14168, .F. ) ;
#19567 = AXIS2_PLACEMENT_3D ( 'NONE', #20150, #296, #2329 ) ;
#19568 = APPROVAL_STATUS ( 'not_yet_approved' ) ;
#19569 = CARTESIAN_POINT ( 'NONE',  ( 0.000000000000000000, -17.30000000000000071, -5.000000000000000000 ) ) ;
#19570 = AXIS2_PLACEMENT_3D ( 'NONE', #14777, #5405, #22012 ) ;
#19571 = EDGE_CURVE ( 'NONE', #357, #11330, #12045, .T. ) ;
#19572 = DIRECTION ( 'NONE',  ( 1.466984912809907930E-16, 2.805478249466195144E-20, 1.000000000000000000 ) ) ;
#19573 = ORIENTED_EDGE ( 'NONE', *, *, #8903, .F. ) ;
#19574 = ADVANCED_FACE ( 'NONE', ( #20923 ), #15461, .F. ) ;
#19575 = EDGE_CURVE ( 'NONE', #15192, #11837, #4666, .T. ) ;
#19576 = ORIENTED_EDGE ( 'NONE', *, *, #18512, .T. ) ;
#19577 = DIRECTION ( 'NONE',  ( 1.749697687228930073E-14, 7.407713590344219741E-14, -1.000000000000000000 ) ) ;
#19578 = DIRECTION ( 'NONE',  ( -0.9730401042858024541, 0.2306359803922080898, 5.959266323858942451E-17 ) ) ;
#19579 = ORIENTED_EDGE ( 'NONE', *, *, #18938, .F. ) ;
#19580 = DIRECTION ( 'NONE',  ( 0.2306359803922084506, 0.9730401042858022320, -5.112869192352694760E-15 ) ) ;
#19581 = DIRECTION ( 'NONE',  ( -0.2306359803922083396, -0.9730401042858023430, -4.336808689942018998E-14 ) ) ;
#19582 = VERTEX_POINT ( 'NONE', #15710 ) ;
#19583 = EDGE_LOOP ( 'NONE', ( #6218, #8852 ) ) ;
#19584 = DATE_TIME_ROLE ( 'classification_date' ) ;
#19585 = AXIS2_PLACEMENT_3D ( 'NONE', #22561, #13544, #20786 ) ;
#19586 = ORIENTED_EDGE ( 'NONE', *, *, #1319, .F. ) ;
#19587 = ORIENTED_EDGE ( 'NONE', *, *, #15091, .F. ) ;
#19588 = CARTESIAN_POINT ( 'NONE',  ( -23.49893655333865894, 22.87624079303418156, 2.499999999999950262 ) ) ;
#19589 = DATE_TIME_ROLE ( 'classification_date' ) ;
#19590 = DIRECTION ( 'NONE',  ( -2.982858504577319616E-17, 2.441916418604790135E-15, 1.000000000000000000 ) ) ;
#19591 = DATE_TIME_ROLE ( 'classification_date' ) ;
#19592 = APPLICATION_CONTEXT ( 'configuration controlled 3d designs of mechanical parts and assemblies' ) ;
#19593 = VECTOR ( 'NONE', #303, 1000.000000000000114 ) ;
#19594 = CIRCLE ( 'NONE', #7834, 2.066999999999997506 ) ;
#19595 =( NAMED_UNIT ( * ) PLANE_ANGLE_UNIT ( ) SI_UNIT ( $, .RADIAN. ) );
#19596 = ADVANCED_FACE ( 'NONE', ( #6437 ), #13814, .T. ) ;
#19597 = CARTESIAN_POINT ( 'NONE',  ( -69.90454993788389970, 6.134066389438220135, 0.7502499999999270308 ) ) ;
#19598 = PERSON_AND_ORGANIZATION ( #11966, #8758 ) ;
#19599 = ORIENTED_EDGE ( 'NONE', *, *, #12062, .F. ) ;
#19600 = DIRECTION ( 'NONE',  ( 0.2306359803922028162, 0.9730401042858035643, -1.412237191019910621E-17 ) ) ;
#19601 = DIRECTION ( 'NONE',  ( 3.764133351409869857E-47, -1.000000000000000000, 4.861311874385510251E-15 ) ) ;
#19602 = ORIENTED_EDGE ( 'NONE', *, *, #3617, .F. ) ;
#19603 = CARTESIAN_POINT ( 'NONE',  ( 53.15246078658950069, 27.48624099592299785, 2.283500000000032948 ) ) ;
#19604 = CARTESIAN_POINT ( 'NONE',  ( -11.34268231757140022, -0.05939068843019999766, 9.040405456159088690E-14 ) ) ;
#19605 = CARTESIAN_POINT ( 'NONE',  ( 35.59419854219520118, 9.774809681453501042, 17.69999999999999929 ) ) ;
#19606 = AXIS2_PLACEMENT_3D ( 'NONE', #6821, #17633, #19179 ) ;
#19607 = EDGE_LOOP ( 'NONE', ( #18426, #17989, #17159, #9865 ) ) ;
#19608 = ORIENTED_EDGE ( 'NONE', *, *, #13329, .F. ) ;
#19609 = DIRECTION ( 'NONE',  ( 0.2306359803922030938, 0.9730401042858035643, -4.741332172907964454E-18 ) ) ;
#19610 = APPROVAL_STATUS ( 'not_yet_approved' ) ;
#19611 = EDGE_CURVE ( 'NONE', #21109, #10345, #6200, .T. ) ;
#19612 = VECTOR ( 'NONE', #15154, 1000.000000000000000 ) ;
#19613 = ORIENTED_EDGE ( 'NONE', *, *, #14009, .F. ) ;
#19614 = VERTEX_POINT ( 'NONE', #4896 ) ;
#19615 = CARTESIAN_POINT ( 'NONE',  ( 119.9163041628193440, 1.024182177979865882, 13.00000000000000000 ) ) ;
#19616 = DIRECTION ( 'NONE',  ( 0.000000000000000000, -1.000000000000000000, 2.081668171172169697E-15 ) ) ;
#19617 = CIRCLE ( 'NONE', #19225, 2.066999999999998838 ) ;
#19618 = DIRECTION ( 'NONE',  ( 3.837966487416234409E-32, -1.216195237911450118E-15, -1.000000000000000000 ) ) ;
#19619 = DATE_AND_TIME ( #16056, #17120 ) ;
#19620 = DIRECTION ( 'NONE',  ( 2.982858504577314686E-17, -2.441916418604790135E-15, -1.000000000000000000 ) ) ;
#19621 = CARTESIAN_POINT ( 'NONE',  ( 36.10037903421270755, -9.768828191507889613, -3.399999999999939959 ) ) ;
#19622 = CIRCLE ( 'NONE', #21878, 3.750000000000000000 ) ;
#19623 =( NAMED_UNIT ( * ) PLANE_ANGLE_UNIT ( ) SI_UNIT ( $, .RADIAN. ) );
#19624 = CONICAL_SURFACE ( 'NONE', #18891, 2.283499999999998753, 0.7853981633974433940 ) ;
#19626 = LINE ( 'NONE', #10866, #17390 ) ;
#19625 = VECTOR ( 'NONE', #16319, 1000.000000000000000 ) ;
#19627 = APPROVAL_STATUS ( 'not_yet_approved' ) ;
#19628 = VECTOR ( 'NONE', #19893, 999.9999999999998863 ) ;
#19629 = CONICAL_SURFACE ( 'NONE', #15438, 2.624999999999998668, 0.4636476090008128104 ) ;
#19630 = DIRECTION ( 'NONE',  ( 0.9730401042858036753, -0.2306359803922031493, 2.804983810440361760E-16 ) ) ;
#19631 = DIRECTION ( 'NONE',  ( 0.9730401042858024541, -0.2306359803922080898, -5.959266323858952312E-17 ) ) ;
#19632 = CARTESIAN_POINT ( 'NONE',  ( 37.27955344062029752, 9.375336445360519022, -27.69000000000049866 ) ) ;
#19633 = LINE ( 'NONE', #12303, #21975 ) ;
#19634 = CARTESIAN_POINT ( 'NONE',  ( 35.54906454756380185, 11.32706792491948278, -27.55602540378494325 ) ) ;
#19635 = ORIENTED_EDGE ( 'NONE', *, *, #11271, .F. ) ;
#19636 = AXIS2_PLACEMENT_3D ( 'NONE', #16561, #18487, #7442 ) ;
#19637 = CARTESIAN_POINT ( 'NONE',  ( 2.664535259100379799E-14, 6.659954201878760116E-16, 2.500000000000000000 ) ) ;
#19638 = UNCERTAINTY_MEASURE_WITH_UNIT (LENGTH_MEASURE( 1.000000000000000082E-05 ), #6700, 'distance_accuracy_value', 'NONE');
#19639 = EDGE_CURVE ( 'NONE', #10034, #17399, #19171, .T. ) ;
#19640 = EDGE_CURVE ( 'NONE', #10837, #1739, #2021, .T. ) ;
#19641 = EDGE_LOOP ( 'NONE', ( #2904, #4739, #12920, #21042 ) ) ;
#19642 = CARTESIAN_POINT ( 'NONE',  ( 35.59419854219520118, 9.774809681453319854, -19.78350000000000009 ) ) ;
#19643 = DIRECTION ( 'NONE',  ( 0.000000000000000000, 0.000000000000000000, 1.000000000000000000 ) ) ;
#19644 = CIRCLE ( 'NONE', #7142, 3.499999999999999112 ) ;
#19645 = ORIENTED_EDGE ( 'NONE', *, *, #20238, .F. ) ;
#19646 = DIRECTION ( 'NONE',  ( -1.534091707905539846E-93, -1.712291624595989929E-31, 1.000000000000000000 ) ) ;
#19647 = CIRCLE ( 'NONE', #3333, 2.009239999999998805 ) ;
#19648 = ORIENTED_EDGE ( 'NONE', *, *, #19251, .T. ) ;
#19649 = CARTESIAN_POINT ( 'NONE',  ( 31.65707447484311743, 2.486356205010160192, -13.00000000000000000 ) ) ;
#19650 = VECTOR ( 'NONE', #19772, 1000.000000000000000 ) ;
#19651 = APPROVAL_STATUS ( 'not_yet_approved' ) ;
#19652 = DIRECTION ( 'NONE',  ( -1.734723475976802677E-14, -1.084202172485501657E-13, 1.000000000000000000 ) ) ;
#19653 = ADVANCED_FACE ( 'NONE', ( #3228 ), #10495, .F. ) ;
#19654 = ADVANCED_FACE ( 'NONE', ( #22693, #11940 ), #2882, .F. ) ;
#19655 = CARTESIAN_POINT ( 'NONE',  ( -30.75845054331819739, -0.1610523420890130064, 2.999000000000090260 ) ) ;
#19656 = DIRECTION ( 'NONE',  ( -0.2306359803922053142, -0.9730401042858028982, 0.000000000000000000 ) ) ;
#19657 = DIRECTION ( 'NONE',  ( 0.000000000000000000, 0.000000000000000000, 1.000000000000000000 ) ) ;
#19658 = CIRCLE ( 'NONE', #12467, 3.499999999999996891 ) ;
#19659 = DIRECTION ( 'NONE',  ( -1.000000000000000000, -6.662112528310618598E-09, 2.269018306577664942E-13 ) ) ;
#19660 = ORIENTED_EDGE ( 'NONE', *, *, #17354, .T. ) ;
#19661 = DIRECTION ( 'NONE',  ( -0.2306359803921919083, -0.9730401042858062288, -4.336808689942036669E-14 ) ) ;
#19662 = CARTESIAN_POINT ( 'NONE',  ( -16.50082286259691955, 23.02797946379192950, -3.750000000000059508 ) ) ;
#19663 = VECTOR ( 'NONE', #1912, 1000.000000000000000 ) ;
#19664 = ORIENTED_EDGE ( 'NONE', *, *, #10946, .F. ) ;
#19665 = DIRECTION ( 'NONE',  ( 1.138590270679730064E-14, 2.220446049251240387E-15, 1.000000000000000000 ) ) ;
#19666 = DIRECTION ( 'NONE',  ( -1.000000000000000000, 1.982541115402065307E-15, 0.000000000000000000 ) ) ;
#19667 = ORIENTED_EDGE ( 'NONE', *, *, #14132, .F. ) ;
#19668 = EDGE_CURVE ( 'NONE', #5242, #1137, #17966, .T. ) ;
#19669 = COORDINATED_UNIVERSAL_TIME_OFFSET ( 0, 0, .AHEAD. ) ;
#19670 = CARTESIAN_POINT ( 'NONE',  ( 62.70840910389689782, 3.348031886875279639, 1.061114750357439988E-14 ) ) ;
#19671 = VERTEX_POINT ( 'NONE', #12500 ) ;
#19672 = ORIENTED_EDGE ( 'NONE', *, *, #7453, .F. ) ;
#19674 = APPROVAL_ROLE ( '' ) ;
#19673 = CC_DESIGN_PERSON_AND_ORGANIZATION_ASSIGNMENT ( #17408, #23078, ( #19087 ) ) ;
#19675 = LINE ( 'NONE', #14218, #21335 ) ;
#19676 = ORIENTED_EDGE ( 'NONE', *, *, #5694, .F. ) ;
#19677 = CC_DESIGN_PERSON_AND_ORGANIZATION_ASSIGNMENT ( #3693, #18187, ( #4728 ) ) ;
#19678 = CARTESIAN_POINT ( 'NONE',  ( 118.4388045014059969, -7.086722380115159758, -19.59999999999999787 ) ) ;
#19679 = APPROVAL_DATE_TIME ( #21561, #12300 ) ;
#19680 = EDGE_CURVE ( 'NONE', #18242, #15192, #6983, .T. ) ;
#19681 = EDGE_CURVE ( 'NONE', #11043, #2245, #11159, .T. ) ;
#19682 = EDGE_CURVE ( 'NONE', #19010, #22465, #14818, .T. ) ;
#19683 = AXIS2_PLACEMENT_3D ( 'NONE', #22474, #2645, #6221 ) ;
#19684 = ADVANCED_FACE ( 'NONE', ( #2224 ), #16394, .T. ) ;
#19685 = FACE_OUTER_BOUND ( 'NONE', #13565, .T. ) ;
#19686 = DIRECTION ( 'NONE',  ( 0.9949874374308234071, 0.09999999677421649025, -2.262079412673754937E-13 ) ) ;
#19687 = AXIS2_PLACEMENT_3D ( 'NONE', #20719, #13486, #17161 ) ;
#19688 = ORIENTED_EDGE ( 'NONE', *, *, #23344, .T. ) ;
#19689 = DIRECTION ( 'NONE',  ( 0.000000000000000000, 0.000000000000000000, 1.000000000000000000 ) ) ;
#19690 = ORIENTED_EDGE ( 'NONE', *, *, #13911, .T. ) ;
#19691 = CARTESIAN_POINT ( 'NONE',  ( 61.45890873801150178, 17.00438549795330090, -13.00000000000000000 ) ) ;
#19692 = FACE_BOUND ( 'NONE', #18401, .T. ) ;
#19693 = ORIENTED_EDGE ( 'NONE', *, *, #22096, .T. ) ;
#19694 = ADVANCED_FACE ( 'NONE', ( #16842 ), #16052, .T. ) ;
#19695 = LINE ( 'NONE', #8554, #911 ) ;
#19696 = LINE ( 'NONE', #7233, #22480 ) ;
#19697 = VERTEX_POINT ( 'NONE', #9617 ) ;
#19698 = ORIENTED_EDGE ( 'NONE', *, *, #7741, .F. ) ;
#19699 = PERSON_AND_ORGANIZATION_ROLE ( 'creator' ) ;
#19700 = ORIENTED_EDGE ( 'NONE', *, *, #21834, .T. ) ;
#19701 = ORIENTED_EDGE ( 'NONE', *, *, #22912, .T. ) ;
#19702 = CARTESIAN_POINT ( 'NONE',  ( -23.49893655333878684, 22.87624079303554581, 2.499999999999900524 ) ) ;
#19703 = CC_DESIGN_SECURITY_CLASSIFICATION ( #6423, ( #23481 ) ) ;
#19704 = APPLICATION_PROTOCOL_DEFINITION ( 'international standard', 'config_control_design', 1994, #473 ) ;
#19705 = VECTOR ( 'NONE', #21071, 1000.000000000000000 ) ;
#19706 = EDGE_CURVE ( 'NONE', #2719, #18769, #12256, .T. ) ;
#19707 = ADVANCED_FACE ( 'NONE', ( #5358 ), #22052, .F. ) ;
#19708 = LINE ( 'NONE', #4990, #4787 ) ;
#19709 = CONTEXT_DEPENDENT_SHAPE_REPRESENTATION ( #654, #2089 ) ;
#19710 = CARTESIAN_POINT ( 'NONE',  ( -15.00000000000000000, -20.00000000000000000, 0.000000000000000000 ) ) ;
#19711 = PERSON_AND_ORGANIZATION ( #11966, #8758 ) ;
#19712 = PRODUCT_DEFINITION_SHAPE ( 'NONE', 'NONE',  #1978 ) ;
#19713 = ORIENTED_EDGE ( 'NONE', *, *, #9417, .T. ) ;
#19714 = AXIS2_PLACEMENT_3D ( 'NONE', #14067, #8614, #23077 ) ;
#19715 = AXIS2_PLACEMENT_3D ( 'NONE', #17247, #11571, #6197 ) ;
#19716 = CARTESIAN_POINT ( 'NONE',  ( -62.94070309524829554, 13.05707373847569919, -5.515665073666220062E-15 ) ) ;
#19717 = AXIS2_PLACEMENT_3D ( 'NONE', #20314, #18428, #7493 ) ;
#19718 = FACE_OUTER_BOUND ( 'NONE', #10724, .T. ) ;
#19719 = VERTEX_POINT ( 'NONE', #7157 ) ;
#19720 = EDGE_CURVE ( 'NONE', #13535, #15230, #4263, .T. ) ;
#19721 = CARTESIAN_POINT ( 'NONE',  ( 52.73786095581300515, -7.648876468381129889, 13.00000000000019895 ) ) ;
#19722 = DIRECTION ( 'NONE',  ( 1.213490492418610097E-15, 4.861311874477940294E-15, 1.000000000000000000 ) ) ;
#19723 = FACE_OUTER_BOUND ( 'NONE', #7557, .T. ) ;
#19724 = ORIENTED_EDGE ( 'NONE', *, *, #12616, .F. ) ;
#19725 = EDGE_LOOP ( 'NONE', ( #8534, #15403, #15254, #1549 ) ) ;
#19726 = FACE_OUTER_BOUND ( 'NONE', #18557, .T. ) ;
#19727 = ORIENTED_EDGE ( 'NONE', *, *, #14344, .T. ) ;
#19728 = AXIS2_PLACEMENT_3D ( 'NONE', #15597, #22835, #8489 ) ;
#19729 = CALENDAR_DATE ( 2026, 31, 10 ) ;
#19730 = ORIENTED_EDGE ( 'NONE', *, *, #3818, .F. ) ;
#19731 = ORIENTED_EDGE ( 'NONE', *, *, #13008, .F. ) ;
#19732 = DIRECTION ( 'NONE',  ( -0.6944962871189167553, 0.7194962871190087039, 0.000000000000000000 ) ) ;
#19733 = DIRECTION ( 'NONE',  ( -0.2306359803922083396, -0.9730401042858023430, -1.333568672157170959E-13 ) ) ;
#19734 = PLANE ( 'NONE',  #430 ) ;
#19735 = MECHANICAL_CONTEXT ( 'NONE', #2142, 'mechanical' ) ;
#19736 = EDGE_CURVE ( 'NONE', #3226, #6720, #20291, .T. ) ;
#19737 = DIRECTION ( 'NONE',  ( 0.000000000000000000, 0.000000000000000000, 1.000000000000000000 ) ) ;
#19738 = LOCAL_TIME ( 14, 11, 27.00000000000000000, #12138 ) ;
#19739 = ADVANCED_FACE ( 'NONE', ( #5133 ), #12388, .T. ) ;
#19740 = CARTESIAN_POINT ( 'NONE',  ( 121.1303491780936099, 5.207460461920199180, 13.00000000000000000 ) ) ;
#19741 = AXIS2_PLACEMENT_3D ( 'NONE', #22251, #2668, #15019 ) ;
#19742 = CARTESIAN_POINT ( 'NONE',  ( 0.000000000000000000, 0.000000000000000000, 0.000000000000000000 ) ) ;
#19743 = AXIS2_PLACEMENT_3D ( 'NONE', #9724, #15511, #13391 ) ;
#19744 = CARTESIAN_POINT ( 'NONE',  ( 45.07211867146960316, 28.08243186520980217, 10.02499999999999858 ) ) ;
#19745 = COORDINATED_UNIVERSAL_TIME_OFFSET ( 0, 0, .AHEAD. ) ;
#19746 = VECTOR ( 'NONE', #7277, 1000.000000000000227 ) ;
#19747 = CARTESIAN_POINT ( 'NONE',  ( 52.05497947389309843, 22.85602965967900246, -2.066999999999965532 ) ) ;
#19748 = CARTESIAN_POINT ( 'NONE',  ( 37.48968750243700043, 22.68571848161319693, -14.15470053837974973 ) ) ;
#19749 = DIRECTION ( 'NONE',  ( 1.040345436475888435E-32, 1.169424102322700040E-16, 1.000000000000000000 ) ) ;
#19750 = APPROVAL_PERSON_ORGANIZATION ( #2735, #16341, #13194 ) ;
#19751 = DIRECTION ( 'NONE',  ( -6.662112528310618598E-09, 1.000000000000000000, -2.081668171172169697E-15 ) ) ;
#19752 = LINE ( 'NONE', #16293, #11860 ) ;
#19753 = APPROVAL_PERSON_ORGANIZATION ( #19388, #3566, #10386 ) ;
#19754 = ORIENTED_EDGE ( 'NONE', *, *, #12480, .T. ) ;
#19755 = DIRECTION ( 'NONE',  ( 1.000000000000000000, 6.662111466122900240E-09, -1.138590272159020020E-14 ) ) ;
#19756 = PRODUCT_DEFINITION ( 'UNKNOWN', '', #11077, #16101 ) ;
#19757 = AXIS2_PLACEMENT_3D ( 'NONE', #8530, #10313, #1604 ) ;
#19758 = VERTEX_POINT ( 'NONE', #19615 ) ;
#19759 = DIRECTION ( 'NONE',  ( 1.329038238457898285E-16, -2.538252868458137019E-14, 1.000000000000000000 ) ) ;
#19760 = CARTESIAN_POINT ( 'NONE',  ( 28.89837840081079889, -1.998294948772169954, 13.00000000000019895 ) ) ;
#19761 = ORIENTED_EDGE ( 'NONE', *, *, #7830, .T. ) ;
#19762 = AXIS2_PLACEMENT_3D ( 'NONE', #23446, #1952, #19779 ) ;
#19763 = DIRECTION ( 'NONE',  ( -1.187319687680499994E-16, -2.805478249478560216E-20, -1.000000000000000000 ) ) ;
#19764 = ORIENTED_EDGE ( 'NONE', *, *, #15327, .T. ) ;
#19765 = DIRECTION ( 'NONE',  ( 0.9730401042858024541, -0.2306359803922080898, -5.959266323858942451E-17 ) ) ;
#19766 = APPROVAL_DATE_TIME ( #23321, #11279 ) ;
#19767 = DIRECTION ( 'NONE',  ( 0.2306359803922033713, 0.9730401042858035643, -4.741332172907925165E-18 ) ) ;
#19768 = PRODUCT_DEFINITION_FORMATION_WITH_SPECIFIED_SOURCE ( 'ANY', '', #8325, .NOT_KNOWN. ) ;
#19769 = LOCAL_TIME ( 14, 11, 27.00000000000000000, #13096 ) ;
#19770 = CARTESIAN_POINT ( 'NONE',  ( 28.89837840081079889, -1.998294948772169954, 13.00000000000019895 ) ) ;
#19771 = EDGE_CURVE ( 'NONE', #9157, #22099, #5805, .T. ) ;
#19772 = DIRECTION ( 'NONE',  ( 0.005235963827110212514, -0.9999862922474493931, -6.182393958678891872E-17 ) ) ;
#19773 = LOCAL_TIME ( 14, 11, 27.00000000000000000, #16223 ) ;
#19774 = APPROVAL_PERSON_ORGANIZATION ( #178, #21957, #12566 ) ;
#19775 = CARTESIAN_POINT ( 'NONE',  ( -14.00000000144740042, -4.350228928435730502, 5.500000000004459544 ) ) ;
#19776 =( REPRESENTATION_RELATIONSHIP ('NONE','NONE', #19303, #16866 ) REPRESENTATION_RELATIONSHIP_WITH_TRANSFORMATION ( #13053 )SHAPE_REPRESENTATION_RELATIONSHIP( ) );
#19777 = FACE_OUTER_BOUND ( 'NONE', #9278, .T. ) ;
#19778 = DIRECTION ( 'NONE',  ( 1.000000000000000000, 9.248967332749676061E-11, -1.127570259384924611E-14 ) ) ;
#19779 = DIRECTION ( 'NONE',  ( -0.9999862922474491711, -0.005235963827128305680, 1.734723475976808327E-16 ) ) ;
#19780 = ORIENTED_EDGE ( 'NONE', *, *, #11742, .T. ) ;
#19781 = SHAPE_REPRESENTATION ( '1602p_c_36', ( #12739 ), #19347 ) ;
#19782 = DIRECTION ( 'NONE',  ( 0.1982893547227609354, 0.8365715274350927766, -0.5107146084542198983 ) ) ;
#19783 = DIRECTION ( 'NONE',  ( 0.000000000000000000, 0.000000000000000000, -1.000000000000000000 ) ) ;
#19784 = ADVANCED_FACE ( 'NONE', ( #4131 ), #19805, .T. ) ;
#19785 = VERTEX_POINT ( 'NONE', #436 ) ;
#19786 = LOCAL_TIME ( 14, 11, 27.00000000000000000, #13571 ) ;
#19787 = CARTESIAN_POINT ( 'NONE',  ( -16.50000000144930112, -4.350228928667009498, -7.999999999996299849 ) ) ;
#19788 = ORIENTED_EDGE ( 'NONE', *, *, #6695, .T. ) ;
#19789 = AXIS2_PLACEMENT_3D ( 'NONE', #11768, #13526, #8302 ) ;
#19790 = CALENDAR_DATE ( 2026, 31, 10 ) ;
#19791 = CARTESIAN_POINT ( 'NONE',  ( -59.86018132287835414, -2.313457456393734901, -5.524798807282839984E-15 ) ) ;
#19792 = ORIENTED_EDGE ( 'NONE', *, *, #8008, .F. ) ;
#19793 = CARTESIAN_POINT ( 'NONE',  ( -20.00000000000000000, -20.00000000000000000, 5.500000000004559020 ) ) ;
#19794 = SECURITY_CLASSIFICATION ( '', '', #4579 ) ;
#19795 = COORDINATED_UNIVERSAL_TIME_OFFSET ( 0, 0, .AHEAD. ) ;
#19796 = APPROVAL_ROLE ( '' ) ;
#19797 = FACE_OUTER_BOUND ( 'NONE', #10666, .T. ) ;
#19798 = EDGE_CURVE ( 'NONE', #16708, #11308, #1550, .T. ) ;
#19799 = APPROVAL_PERSON_ORGANIZATION ( #13313, #9224, #6301 ) ;
#19800 = CARTESIAN_POINT ( 'NONE',  ( -2.291879384893320104, 10.94490600546980019, -2.500000000000000000 ) ) ;
#19801 = AXIS2_PLACEMENT_3D ( 'NONE', #9180, #16525, #21872 ) ;
#19802 = ORIENTED_EDGE ( 'NONE', *, *, #21592, .T. ) ;
#19803 = CARTESIAN_POINT ( 'NONE',  ( 2.664535259100379799E-14, -1.554450629062440126E-15, 2.500000000000000000 ) ) ;
#19804 = CC_DESIGN_PERSON_AND_ORGANIZATION_ASSIGNMENT ( #4961, #12229, ( #8018 ) ) ;
#19805 = CONICAL_SURFACE ( 'NONE', #6159, 5.086751345948125724, 1.047197551196598297 ) ;
#19806 = AXIS2_PLACEMENT_3D ( 'NONE', #4946, #10199, #13859 ) ;
#19807 = ORIENTED_EDGE ( 'NONE', *, *, #10459, .T. ) ;
#19808 = APPROVAL_PERSON_ORGANIZATION ( #194, #11838, #16472 ) ;
#19809 = LINE ( 'NONE', #7350, #5166 ) ;
#19810 = DIRECTION ( 'NONE',  ( 0.000000000000000000, 0.000000000000000000, -1.000000000000000000 ) ) ;
#19811 = CARTESIAN_POINT ( 'NONE',  ( 36.79228697538940196, -6.849707878650479920, -3.400000000000049649 ) ) ;
#19812 = EDGE_LOOP ( 'NONE', ( #12869, #19135, #12281, #5132 ) ) ;
#19813 = EDGE_CURVE ( 'NONE', #22408, #8421, #20570, .T. ) ;
#19814 = EDGE_CURVE ( 'NONE', #9733, #306, #10231, .T. ) ;
#19815 = CIRCLE ( 'NONE', #21697, 2.499999999999998668 ) ;
#19816 = CARTESIAN_POINT ( 'NONE',  ( 35.59419854219520118, 9.774809681453469068, 10.74538000000019977 ) ) ;
#19817 = DIRECTION ( 'NONE',  ( -0.9730401042858022320, 0.2306359803922080343, 5.959266323858941219E-17 ) ) ;
#19818 = ORIENTED_EDGE ( 'NONE', *, *, #23132, .F. ) ;
#19819 = DATE_AND_TIME ( #14238, #14459 ) ;
#19820 = LOCAL_TIME ( 14, 11, 27.00000000000000000, #2594 ) ;
#19821 = EDGE_LOOP ( 'NONE', ( #15728, #16391, #8409, #4952, #9789, #11721 ) ) ;
#19822 = VERTEX_POINT ( 'NONE', #674 ) ;
#19823 = CARTESIAN_POINT ( 'NONE',  ( 35.09747506357100377, 11.43410645592859964, 28.46999999999999886 ) ) ;
#19824 = APPROVAL_STATUS ( 'not_yet_approved' ) ;
#19825 = CIRCLE ( 'NONE', #15261, 2.600000000000000089 ) ;
#19826 = CIRCLE ( 'NONE', #21352, 6.499999999999998224 ) ;
#19827 = DIRECTION ( 'NONE',  ( 2.270069654138870255E-15, 1.000000000000000000, 7.035747901516317327E-77 ) ) ;
#19828 = APPROVAL_DATE_TIME ( #14482, #17650 ) ;
#19829 = DIRECTION ( 'NONE',  ( -6.662160722082822564E-09, 1.000000000000000000, -2.523234146875356491E-15 ) ) ;
#19830 = CIRCLE ( 'NONE', #7693, 4.250000000000000000 ) ;
#19831 = EDGE_CURVE ( 'NONE', #12125, #10900, #18975, .T. ) ;
#19832 = SHAPE_REPRESENTATION_RELATIONSHIP ( 'NONE' , 'NONE' ,  #19781, #10822 ) ;
#19834 = AXIS2_PLACEMENT_3D ( 'NONE', #23262, #91, #1645 ) ;
#19833 = CARTESIAN_POINT ( 'NONE',  ( 120.3930287342899987, 3.035456073538439714, -13.00000000000000000 ) ) ;
#19835 = AXIS2_PLACEMENT_3D ( 'NONE', #6279, #18881, #11762 ) ;
#19836 = APPROVAL ( #4869, 'UNSPECIFIED' ) ;
#19837 = COORDINATED_UNIVERSAL_TIME_OFFSET ( 0, 0, .AHEAD. ) ;
#19838 = CC_DESIGN_APPROVAL ( #12579, ( #10854 ) ) ;
#19839 = CC_DESIGN_PERSON_AND_ORGANIZATION_ASSIGNMENT ( #6890, #8313, ( #6875 ) ) ;
#19840 = ORIENTED_EDGE ( 'NONE', *, *, #13762, .T. ) ;
#19841 = CARTESIAN_POINT ( 'NONE',  ( 8.284960688207149815, -8.610885316305250115, 25.00000000000000000 ) ) ;
#19842 = VECTOR ( 'NONE', #12243, 1000.000000000000000 ) ;
#19843 = CARTESIAN_POINT ( 'NONE',  ( -20.00000000000190070, -20.00000000000000000, -8.499999999995459632 ) ) ;
#19844 = ORIENTED_EDGE ( 'NONE', *, *, #10277, .F. ) ;
#19845 = EDGE_CURVE ( 'NONE', #8301, #4246, #8055, .T. ) ;
#19846 = VECTOR ( 'NONE', #5969, 999.9999999999998863 ) ;
#19847 = EDGE_CURVE ( 'NONE', #21038, #7183, #12975, .T. ) ;
#19848 = DIRECTION ( 'NONE',  ( -0.2306359803922040930, -0.9730401042858032312, 4.616450158279817280E-15 ) ) ;
#19849 = CIRCLE ( 'NONE', #8483, 2.749999999999999112 ) ;
#19850 = DIRECTION ( 'NONE',  ( -0.07397971354964476276, -0.9972597464969256142, 2.428612866367529538E-15 ) ) ;
#19851 = FACE_BOUND ( 'NONE', #711, .T. ) ;
#19852 = ORIENTED_EDGE ( 'NONE', *, *, #8537, .T. ) ;
#19853 = ORIENTED_EDGE ( 'NONE', *, *, #14630, .F. ) ;
#19854 = CARTESIAN_POINT ( 'NONE',  ( 61.45890873801150178, 17.00438549795330090, -13.00000000000000000 ) ) ;
#19855 = EDGE_LOOP ( 'NONE', ( #11616, #18808, #4412, #3715 ) ) ;
#19856 = PERSON_AND_ORGANIZATION_ROLE ( 'design_owner' ) ;
#19857 = ORIENTED_EDGE ( 'NONE', *, *, #18959, .F. ) ;
#19858 = ORIENTED_EDGE ( 'NONE', *, *, #3498, .F. ) ;
#19859 = DIRECTION ( 'NONE',  ( 0.9730401042858035643, -0.2306359803922028717, -5.432877459303547053E-17 ) ) ;
#19860 = DIRECTION ( 'NONE',  ( -8.623081276789554834E-17, -1.054188326053478339E-16, -1.000000000000000000 ) ) ;
#19861 = CIRCLE ( 'NONE', #6973, 2.500000000000000000 ) ;
#19862 = CARTESIAN_POINT ( 'NONE',  ( 28.67817383939640052, -0.7594070262927730131, -15.00000000000039968 ) ) ;
#19863 = APPROVAL_STATUS ( 'not_yet_approved' ) ;
#19864 = DIRECTION ( 'NONE',  ( -0.2306359803922031215, -0.9730401042858034533, 5.121148285185918258E-15 ) ) ;
#19865 = APPROVAL_PERSON_ORGANIZATION ( #5220, #6447, #23266 ) ;
#19866 = VECTOR ( 'NONE', #17182, 1000.000000000000227 ) ;
#19867 = DIRECTION ( 'NONE',  ( -0.2306359803922028717, -0.9730401042858034533, 1.407521210652564497E-17 ) ) ;
#19868 = AXIS2_PLACEMENT_3D ( 'NONE', #8905, #21700, #1749 ) ;
#19869 = EDGE_CURVE ( 'NONE', #17589, #20801, #15264, .T. ) ;
#19870 = VECTOR ( 'NONE', #5664, 1000.000000000000000 ) ;
#19871 = CARTESIAN_POINT ( 'NONE',  ( 0.000000000000000000, 0.000000000000000000, 0.000000000000000000 ) ) ;
#19872 = CARTESIAN_POINT ( 'NONE',  ( -13.66075527208050033, 1.277470069177119916, -5.000000000000000000 ) ) ;
#19873 = APPROVAL_ROLE ( '' ) ;
#19874 = ADVANCED_FACE ( 'NONE', ( #11991 ), #6147, .T. ) ;
#19875 = DIRECTION ( 'NONE',  ( 3.210834492194344756E-17, -2.441916418604790135E-15, -1.000000000000000000 ) ) ;
#19876 = DIRECTION ( 'NONE',  ( 5.798605125234323991E-17, -1.374421231021384554E-17, 1.000000000000000000 ) ) ;
#19877 = EDGE_CURVE ( 'NONE', #17890, #8468, #13276, .T. ) ;
#19878 = CARTESIAN_POINT ( 'NONE',  ( -32.64674982798959491, 7.329300507370480666, 3.750000000000000000 ) ) ;
#19879 = CARTESIAN_POINT ( 'NONE',  ( 27.03882233449094841, -4.640652085158520457, -20.00000000000000000 ) ) ;
#19880 = ADVANCED_FACE ( 'NONE', ( #13512 ), #914, .F. ) ;
#19881 = LINE ( 'NONE', #3480, #22445 ) ;
#19882 = EDGE_LOOP ( 'NONE', ( #6466, #8457 ) ) ;
#19883 = AXIS2_PLACEMENT_3D ( 'NONE', #6048, #13302, #4278 ) ;
#19884 = CARTESIAN_POINT ( 'NONE',  ( -17.50000000397400157, 22.95208920922877738, -5.499999999996137312 ) ) ;
#19885 = ORIENTED_EDGE ( 'NONE', *, *, #9141, .F. ) ;
#19886 = CARTESIAN_POINT ( 'NONE',  ( 35.59419854219520118, 9.774809681453501042, 17.69999999999999929 ) ) ;
#19887 = CYLINDRICAL_SURFACE ( 'NONE', #18583, 6.500000000000000888 ) ;
#19888 = ORIENTED_EDGE ( 'NONE', *, *, #22449, .T. ) ;
#19889 = FACE_OUTER_BOUND ( 'NONE', #8611, .T. ) ;
#19890 = ORIENTED_EDGE ( 'NONE', *, *, #4722, .F. ) ;
#19891 = LINE ( 'NONE', #3614, #18492 ) ;
#19892 = CALENDAR_DATE ( 2026, 31, 10 ) ;
#19893 = DIRECTION ( 'NONE',  ( 0.9730401042858036753, -0.2306359803922028995, -5.432877459303547669E-17 ) ) ;
#19894 =( NAMED_UNIT ( * ) SI_UNIT ( $, .STERADIAN. ) SOLID_ANGLE_UNIT ( ) );
#19895 = CARTESIAN_POINT ( 'NONE',  ( 27.54697342219713718, -5.531877349647952080, -13.00000000000039968 ) ) ;
#19896 = CC_DESIGN_PERSON_AND_ORGANIZATION_ASSIGNMENT ( #6906, #21723, ( #15912 ) ) ;
#19897 = CARTESIAN_POINT ( 'NONE',  ( 52.05497947389309843, 22.85602965967900246, 3.416161896595049310E-14 ) ) ;
#19898 = EDGE_CURVE ( 'NONE', #7665, #7533, #20992, .T. ) ;
#19899 = LINE ( 'NONE', #7086, #519 ) ;
#19900 = CARTESIAN_POINT ( 'NONE',  ( 63.71761976613755962, -9.737513338266090557, 1.037827268014797219E-14 ) ) ;
#19901 = CARTESIAN_POINT ( 'NONE',  ( -23.50000000000000000, -20.00000000000000000, -1.084773659275596300E-61 ) ) ;
#19902 = DESIGN_CONTEXT ( 'detailed design', #16259, 'design' ) ;
#19903 = DIRECTION ( 'NONE',  ( -0.9730401042858035643, 0.2306359803922028717, -2.740969466505749044E-16 ) ) ;
#19904 = ORIENTED_EDGE ( 'NONE', *, *, #740, .F. ) ;
#19905 = CARTESIAN_POINT ( 'NONE',  ( 122.4288069621910040, 9.746871424029270869, 10.02499999999999858 ) ) ;
#19906 = DIRECTION ( 'NONE',  ( -0.8823529412199823119, 0.4705882352125332901, 1.992040791580033901E-13 ) ) ;
#19907 = EDGE_LOOP ( 'NONE', ( #8889, #19226 ) ) ;
#19908 = ORIENTED_EDGE ( 'NONE', *, *, #20592, .T. ) ;
#19909 = DIRECTION ( 'NONE',  ( -6.662160722082822564E-09, 1.000000000000000000, -2.523234146875356491E-15 ) ) ;
#19910 = DIRECTION ( 'NONE',  ( -1.466984912809907930E-16, -2.805478249466195144E-20, -1.000000000000000000 ) ) ;
#19911 = EDGE_LOOP ( 'NONE', ( #4322, #1321, #8087, #21647 ) ) ;
#19912 = APPLICATION_CONTEXT ( 'configuration controlled 3d designs of mechanical parts and assemblies' ) ;
#19913 = AXIS2_PLACEMENT_3D ( 'NONE', #1873, #21852, #21962 ) ;
#19914 = COORDINATED_UNIVERSAL_TIME_OFFSET ( 0, 0, .AHEAD. ) ;
#19915 = CARTESIAN_POINT ( 'NONE',  ( -59.85533902005759899, -24.86725927682059734, -5.000000000000000000 ) ) ;
#19916 = ADVANCED_FACE ( 'NONE', ( #8291 ), #6386, .T. ) ;
#19917 = ORIENTED_EDGE ( 'NONE', *, *, #21765, .F. ) ;
#19918 = CARTESIAN_POINT ( 'NONE',  ( 5.750000000000139444, -20.33108891324529921, -5.000000000000000000 ) ) ;
#19919 = PERSON_AND_ORGANIZATION_ROLE ( 'creator' ) ;
#19920 = PRODUCT ( '1602p_c_17', '1602p_c_17', '', ( #19735 ) ) ;
#19921 = DIRECTION ( 'NONE',  ( -0.2306359803922019835, -0.9730401042858037863, 4.163336342344336238E-15 ) ) ;
#19922 = AXIS2_PLACEMENT_3D ( 'NONE', #12230, #22763, #19117 ) ;
#19923 =( BOUNDED_CURVE ( )  B_SPLINE_CURVE ( 2, ( #10215, #17571, #12116 ),
 .UNSPECIFIED., .F., .F. ) 
 B_SPLINE_CURVE_WITH_KNOTS ( ( 3, 3 ),
 ( 0.000000000000000000, 0.2928548593876180162 ),
 .UNSPECIFIED. ) 
 CURVE ( )  GEOMETRIC_REPRESENTATION_ITEM ( )  RATIONAL_B_SPLINE_CURVE ( ( 1.000000000000000000, 1.037954849302049842, 1.000000000000000000 ) ) 
 REPRESENTATION_ITEM ( '' )  );
#19924 = DIRECTION ( 'NONE',  ( 6.281952996264290168E-17, 4.969341027148640384E-15, 1.000000000000000000 ) ) ;
#19925 = ORIENTED_EDGE ( 'NONE', *, *, #7120, .T. ) ;
#19926 = DIRECTION ( 'NONE',  ( 0.000000000000000000, 1.000000000000000000, 0.000000000000000000 ) ) ;
#19927 = ORIENTED_EDGE ( 'NONE', *, *, #11031, .F. ) ;
#19928 = CARTESIAN_POINT ( 'NONE',  ( 37.01481097301077483, 22.79827665208033238, 15.00000000000000178 ) ) ;
#19929 = LINE ( 'NONE', #10462, #37 ) ;
#19930 = FACE_OUTER_BOUND ( 'NONE', #16274, .T. ) ;
#19931 = VERTEX_POINT ( 'NONE', #16952 ) ;
#19932 = LINE ( 'NONE', #10931, #20240 ) ;
#19933 = LINE ( 'NONE', #5319, #4691 ) ;
#19934 = ORIENTED_EDGE ( 'NONE', *, *, #19242, .T. ) ;
#19935 = APPROVAL_DATE_TIME ( #23258, #11875 ) ;
#19936 = ADVANCED_FACE ( 'NONE', ( #19210 ), #3126, .T. ) ;
#19937 = VERTEX_POINT ( 'NONE', #4375 ) ;
#19938 = CIRCLE ( 'NONE', #19567, 5.000000000000000000 ) ;
#19939 = ORIENTED_EDGE ( 'NONE', *, *, #950, .F. ) ;
#19940 = DIRECTION ( 'NONE',  ( -1.000000000000000000, 0.000000000000000000, 0.000000000000000000 ) ) ;
#19941 = PERSON_AND_ORGANIZATION ( #11966, #8758 ) ;
#19942 = VECTOR ( 'NONE', #2117, 999.9999999999998863 ) ;
#19943 = DIRECTION ( 'NONE',  ( 4.027614241767943373E-31, 2.300154215587010080E-15, 1.000000000000000000 ) ) ;
#19944 = PERSON_AND_ORGANIZATION_ROLE ( 'classification_officer' ) ;
#19945 = DIRECTION ( 'NONE',  ( 3.525869238601989755E-16, 1.745928279345489864E-15, -1.000000000000000000 ) ) ;
#19946 = EDGE_CURVE ( 'NONE', #21240, #22662, #5031, .T. ) ;
#19947 = EDGE_CURVE ( 'NONE', #13864, #11195, #13743, .T. ) ;
#19948 =( LENGTH_UNIT ( ) NAMED_UNIT ( * ) SI_UNIT ( .MILLI., .METRE. ) );
#19949 = DIRECTION ( 'NONE',  ( 0.005235963827117092427, -0.9999862922474493931, -2.636227439667000721E-16 ) ) ;
#19950 = APPROVAL_ROLE ( '' ) ;
#19951 = ORIENTED_EDGE ( 'NONE', *, *, #5888, .T. ) ;
#19952 = LINE ( 'NONE', #5230, #9007 ) ;
#19953 = VERTEX_POINT ( 'NONE', #6501 ) ;
#19954 = AXIS2_PLACEMENT_3D ( 'NONE', #21246, #8569, #12022 ) ;
#19955 = CARTESIAN_POINT ( 'NONE',  ( -24.86147400983239919, -14.96352599016710094, 5.000000000000000000 ) ) ;
#19956 = CARTESIAN_POINT ( 'NONE',  ( -19.49999999982379961, -0.1021026942259700004, -2.500000000000090150 ) ) ;
#19957 = CARTESIAN_POINT ( 'NONE',  ( 117.1933702072879981, -12.34113894325840022, -19.59999999999999787 ) ) ;
#19958 = VERTEX_POINT ( 'NONE', #13629 ) ;
#19959 = VERTEX_POINT ( 'NONE', #9843 ) ;
#19960 = DIRECTION ( 'NONE',  ( 0.7071067811865476838, -1.387778780781444689E-15, 0.7071067811865473507 ) ) ;
#19961 = EDGE_LOOP ( 'NONE', ( #11425, #152 ) ) ;
#19962 = DATE_AND_TIME ( #12730, #3802 ) ;
#19963 = EDGE_CURVE ( 'NONE', #11012, #11097, #11751, .T. ) ;
#19964 = EDGE_LOOP ( 'NONE', ( #4772, #14474 ) ) ;
#19965 = EDGE_LOOP ( 'NONE', ( #21463, #10467, #11693, #10634, #821 ) ) ;
#19966 = DIRECTION ( 'NONE',  ( -0.7070970883417637687, -0.003702385528188433840, 0.7071067811865477948 ) ) ;
#19967 = DIRECTION ( 'NONE',  ( -0.4865200521429013936, 0.1153179901961013387, -0.8660254037844388186 ) ) ;
#19968 = PERSON_AND_ORGANIZATION_ROLE ( 'classification_officer' ) ;
#19969 = PLANE ( 'NONE',  #12024 ) ;
#19970 = CC_DESIGN_DATE_AND_TIME_ASSIGNMENT ( #15853, #18953, ( #15292 ) ) ;
#19971 = CIRCLE ( 'NONE', #1746, 9.000000000000003553 ) ;
#19972 = CC_DESIGN_DATE_AND_TIME_ASSIGNMENT ( #21339, #10908, ( #6637 ) ) ;
#19973 = DIRECTION ( 'NONE',  ( -0.9730401042858022320, 0.2306359803922080343, 5.959266323858941219E-17 ) ) ;
#19974 = EDGE_CURVE ( 'NONE', #14240, #14375, #10205, .T. ) ;
#19975 = ADVANCED_FACE ( 'NONE', ( #20514 ), #17548, .T. ) ;
#19976 = PRODUCT_RELATED_PRODUCT_CATEGORY ( 'detail', '', ( #15912 ) ) ;
#19977 = EDGE_LOOP ( 'NONE', ( #1671, #20230, #6397, #16559 ) ) ;
#19978 = DIRECTION ( 'NONE',  ( 0.9730401042858036753, -0.2306359803922028995, -5.432877459303547669E-17 ) ) ;
#19979 = PERSON_AND_ORGANIZATION_ROLE ( 'creator' ) ;
#19980 = CYLINDRICAL_SURFACE ( 'NONE', #18220, 3.499999999999999556 ) ;
#19981 = DIRECTION ( 'NONE',  ( -0.9730401042858036753, 0.2306359803922031493, -2.804983810440356829E-16 ) ) ;
#19982 = DIRECTION ( 'NONE',  ( 1.000000000000000000, -8.896220237034308570E-17, 0.000000000000000000 ) ) ;
#19983 = AXIS2_PLACEMENT_3D ( 'NONE', #17409, #15618, #11970 ) ;
#19984 = CARTESIAN_POINT ( 'NONE',  ( -27.39120887301850260, 6.327965799971409844, 2.500000000000000000 ) ) ;
#19985 = CIRCLE ( 'NONE', #9769, 2.499999999999999112 ) ;
#19986 = DIRECTION ( 'NONE',  ( -0.9080618652418041004, 0.4188360644614733674, -1.040834085574019418E-15 ) ) ;
#19987 = ORIENTED_EDGE ( 'NONE', *, *, #2811, .F. ) ;
#19988 = DIRECTION ( 'NONE',  ( 0.2306359803922085339, 0.9730401042858022320, 0.000000000000000000 ) ) ;
#19989 = EDGE_CURVE ( 'NONE', #11267, #17345, #17911, .T. ) ;
#19990 = VERTEX_POINT ( 'NONE', #2476 ) ;
#19991 = CARTESIAN_POINT ( 'NONE',  ( -27.00000000000000000, -28.60000000000000142, 19.00000000000000000 ) ) ;
#19992 = LINE ( 'NONE', #21877, #16285 ) ;
#19993 = ORIENTED_EDGE ( 'NONE', *, *, #13957, .T. ) ;
#19994 = CARTESIAN_POINT ( 'NONE',  ( -12.50000000434390124, 26.95208919326699970, -5.499999999997269740 ) ) ;
#19995 = ORIENTED_EDGE ( 'NONE', *, *, #9729, .F. ) ;
#19996 = DIRECTION ( 'NONE',  ( 0.000000000000000000, 0.000000000000000000, 1.000000000000000000 ) ) ;
#19997 = CIRCLE ( 'NONE', #2557, 0.4000000000000001887 ) ;
#19998 = PERSON_AND_ORGANIZATION ( #11966, #8758 ) ;
#19999 = CARTESIAN_POINT ( 'NONE',  ( -9.489957111606940998, 28.27083100358139944, -2.500000000000000000 ) ) ;
#20000 = EDGE_CURVE ( 'NONE', #4506, #14758, #23100, .T. ) ;
#20001 = AXIS2_PLACEMENT_3D ( 'NONE', #21924, #72, #14458 ) ;
#20002 = AXIS2_PLACEMENT_3D ( 'NONE', #17648, #16309, #17871 ) ;
#20003 = ADVANCED_FACE ( 'NONE', ( #21557 ), #1489, .T. ) ;
#20004 = AXIS2_PLACEMENT_3D ( 'NONE', #15916, #5120, #10951 ) ;
#20005 =( LENGTH_UNIT ( ) NAMED_UNIT ( * ) SI_UNIT ( .MILLI., .METRE. ) );
#20006 = CYLINDRICAL_SURFACE ( 'NONE', #16417, 2.500999999999959922 ) ;
#20007 = CYLINDRICAL_SURFACE ( 'NONE', #9026, 2.067000000000000171 ) ;
#20008 = DIRECTION ( 'NONE',  ( 0.000000000000000000, 0.000000000000000000, 1.000000000000000000 ) ) ;
#20009 = CARTESIAN_POINT ( 'NONE',  ( -22.50000000000130029, -20.00000001665528160, -5.499999999994901856 ) ) ;
#20010 = CARTESIAN_POINT ( 'NONE',  ( 36.89121352362742101, 22.27682603178731924, -11.00000000000049738 ) ) ;
#20011 = LINE ( 'NONE', #162, #202 ) ;
#20012 = LINE ( 'NONE', #5407, #17055 ) ;
#20013 = CIRCLE ( 'NONE', #15847, 2.499999999999998668 ) ;
#20014 = DIRECTION ( 'NONE',  ( 5.798605125234323991E-17, -1.374421231021384554E-17, 1.000000000000000000 ) ) ;
#20015 = DIRECTION ( 'NONE',  ( -0.2306359803922029550, -0.9730401042858035643, 4.741332172907960602E-18 ) ) ;
#20016 = VERTEX_POINT ( 'NONE', #17673 ) ;
#20017 = AXIS2_PLACEMENT_3D ( 'NONE', #14310, #9205, #16439 ) ;
#20018 = ORIENTED_EDGE ( 'NONE', *, *, #17193, .T. ) ;
#20019 = PLANE ( 'NONE',  #1231 ) ;
#20020 = AXIS2_PLACEMENT_3D ( 'NONE', #7425, #8734, #12535 ) ;
#20021 = CARTESIAN_POINT ( 'NONE',  ( -2.500000000000012434, -17.29999999999999361, 2.500000000000000000 ) ) ;
#20022 = ORIENTED_EDGE ( 'NONE', *, *, #9060, .T. ) ;
#20023 = CARTESIAN_POINT ( 'NONE',  ( 120.6036919168680015, 2.985523383783529994, -13.00000000000000000 ) ) ;
#20024 = ORIENTED_EDGE ( 'NONE', *, *, #5172, .T. ) ;
#20025 = CARTESIAN_POINT ( 'NONE',  ( 99.36449593087139931, -18.18675627898399583, 3.528131999253151732E-14 ) ) ;
#20026 = ADVANCED_FACE ( 'NONE', ( #10669, #1612 ), #14328, .T. ) ;
#20027 = PERSON_AND_ORGANIZATION ( #11966, #8758 ) ;
#20028 = EDGE_CURVE ( 'NONE', #1580, #12377, #1268, .T. ) ;
#20029 = APPROVAL_STATUS ( 'not_yet_approved' ) ;
#20030 = AXIS2_PLACEMENT_3D ( 'NONE', #22431, #6174, #13426 ) ;
#20031 = DIRECTION ( 'NONE',  ( 0.7273594590164591533, -0.6862566701892842680, 3.292724291071139008E-15 ) ) ;
#20032 = VECTOR ( 'NONE', #7857, 999.9999999999998863 ) ;
#20033 = DIRECTION ( 'NONE',  ( -0.2306359803922025109, -0.9730401042858035643, 5.112869192352692394E-15 ) ) ;
#20034 = ORIENTED_EDGE ( 'NONE', *, *, #20598, .F. ) ;
#20035 = DIRECTION ( 'NONE',  ( -0.9997648976141043642, -0.02168293104402130300, 0.000000000000000000 ) ) ;
#20036 = ORIENTED_EDGE ( 'NONE', *, *, #1863, .T. ) ;
#20037 = CARTESIAN_POINT ( 'NONE',  ( -20.00000000397360012, 22.95208919256889857, -3.750000000000000000 ) ) ;
#20038 = CARTESIAN_POINT ( 'NONE',  ( -20.80722593534541076, 19.54644882756858593, -5.432327950763541660E-15 ) ) ;
#20039 = DIRECTION ( 'NONE',  ( -1.227507208848341976E-15, -4.920447605136010024E-15, -1.000000000000000000 ) ) ;
#20040 = ORIENTED_EDGE ( 'NONE', *, *, #13013, .F. ) ;
#20041 = COORDINATED_UNIVERSAL_TIME_OFFSET ( 0, 0, .AHEAD. ) ;
#20042 = CARTESIAN_POINT ( 'NONE',  ( -27.00000000000000000, -27.34999999999999787, -6.250000000000000000 ) ) ;
#20043 = EDGE_LOOP ( 'NONE', ( #22724, #4767, #961, #1298, #21237, #2222 ) ) ;
#20044 = PERSON_AND_ORGANIZATION_ROLE ( 'creator' ) ;
#20045 = VERTEX_POINT ( 'NONE', #14096 ) ;
#20046 = ORIENTED_EDGE ( 'NONE', *, *, #20362, .T. ) ;
#20047 = CARTESIAN_POINT ( 'NONE',  ( -26.00000000397269773, 22.95208919201850151, 5.500000000004529710 ) ) ;
#20048 = AXIS2_PLACEMENT_3D ( 'NONE', #20217, #9660, #2511 ) ;
#20049 = CALENDAR_DATE ( 2026, 31, 10 ) ;
#20050 = CARTESIAN_POINT ( 'NONE',  ( 122.7747609327790030, 11.20643158045800014, 9.133960000000000079 ) ) ;
#20051 =( BOUNDED_CURVE ( )  B_SPLINE_CURVE ( 2, ( #13188, #4152, #11423 ),
 .UNSPECIFIED., .F., .F. ) 
 B_SPLINE_CURVE_WITH_KNOTS ( ( 3, 3 ),
 ( 0.000000000000000000, 0.5842180690389588982 ),
 .UNSPECIFIED. ) 
 CURVE ( )  GEOMETRIC_REPRESENTATION_ITEM ( )  RATIONAL_B_SPLINE_CURVE ( ( 1.000000000000000000, 1.154700538379249908, 1.000000000000000000 ) ) 
 REPRESENTATION_ITEM ( '' )  );
#20052 = FACE_OUTER_BOUND ( 'NONE', #4314, .T. ) ;
#20053 = EDGE_CURVE ( 'NONE', #15533, #21157, #19675, .T. ) ;
#20054 = DIRECTION ( 'NONE',  ( -0.9730401042858024541, 0.2306359803922080898, 5.959266323858942451E-17 ) ) ;
#20055 = ADVANCED_FACE ( 'NONE', ( #23342 ), #18020, .F. ) ;
#20056 = ADVANCED_FACE ( 'NONE', ( #8536 ), #19448, .F. ) ;
#20057 = DATE_AND_TIME ( #12936, #15167 ) ;
#20058 = ORIENTED_EDGE ( 'NONE', *, *, #23202, .T. ) ;
#20059 = PLANE ( 'NONE',  #8792 ) ;
#20060 = EDGE_LOOP ( 'NONE', ( #7950, #282 ) ) ;
#20061 = DIRECTION ( 'NONE',  ( -0.9730401042858023430, 0.2306359803922080620, 5.959266323858944916E-17 ) ) ;
#20062 = LINE ( 'NONE', #220, #8126 ) ;
#20063 = FACE_BOUND ( 'NONE', #16567, .T. ) ;
#20064 = ORIENTED_EDGE ( 'NONE', *, *, #20637, .T. ) ;
#20065 = CC_DESIGN_SECURITY_CLASSIFICATION ( #6812, ( #23486 ) ) ;
#20066 = ORIENTED_EDGE ( 'NONE', *, *, #498, .F. ) ;
#20068 = DIRECTION ( 'NONE',  ( 2.269747459789000104E-13, 2.220446049250330436E-15, 1.000000000000000000 ) ) ;
#20067 = AXIS2_PLACEMENT_3D ( 'NONE', #1927, #9068, #24 ) ;
#20069 = EDGE_LOOP ( 'NONE', ( #21449, #19888 ) ) ;
#20070 = ADVANCED_FACE ( 'NONE', ( #15875 ), #12558, .T. ) ;
#20071 = EDGE_CURVE ( 'NONE', #10214, #6518, #3053, .T. ) ;
#20072 = APPROVAL_DATE_TIME ( #116, #20557 ) ;
#20073 = ORIENTED_EDGE ( 'NONE', *, *, #545, .T. ) ;
#20074 = ORIENTED_EDGE ( 'NONE', *, *, #21803, .F. ) ;
#20075 = DIRECTION ( 'NONE',  ( -0.9730401042858024541, 0.2306359803922080898, 5.959266323858942451E-17 ) ) ;
#20076 = CARTESIAN_POINT ( 'NONE',  ( 2.169175203825779885, 15.45758013577720114, -4.500000000000000000 ) ) ;
#20077 = APPROVAL_ROLE ( '' ) ;
#20078 = LINE ( 'NONE', #16168, #15682 ) ;
#20079 = DIRECTION ( 'NONE',  ( 0.005235963827121942714, -0.9999862922474493931, -2.738609489598291197E-14 ) ) ;
#20080 = AXIS2_PLACEMENT_3D ( 'NONE', #19742, #15938, #21755 ) ;
#20081 = AXIS2_PLACEMENT_3D ( 'NONE', #20544, #20428, #4158 ) ;
#20082 = ORIENTED_EDGE ( 'NONE', *, *, #23018, .F. ) ;
#20083 = DIRECTION ( 'NONE',  ( -0.2306359803922102825, -0.9730401042858017879, 4.857225732735058287E-15 ) ) ;
#20084 = EDGE_CURVE ( 'NONE', #8301, #8641, #6862, .T. ) ;
#20085 = APPROVAL_ROLE ( '' ) ;
#20086 = VERTEX_POINT ( 'NONE', #12443 ) ;
#20088 = DIRECTION ( 'NONE',  ( 0.1153179901961009640, 0.4865200521429018377, -0.8660254037844385966 ) ) ;
#20087 = VECTOR ( 'NONE', #13941, 1000.000000000000000 ) ;
#20089 = DIRECTION ( 'NONE',  ( 0.9730401042858036753, -0.2306359803922031493, -5.432877459303553216E-17 ) ) ;
#20090 = CC_DESIGN_PERSON_AND_ORGANIZATION_ASSIGNMENT ( #10885, #9195, ( #20819 ) ) ;
#20091 = CARTESIAN_POINT ( 'NONE',  ( 34.14207834813670672, 22.29249582057180135, -11.00000000000049916 ) ) ;
#20092 = DIRECTION ( 'NONE',  ( 1.000000000000000000, 0.000000000000000000, 0.000000000000000000 ) ) ;
#20093 = APPROVAL ( #14440, 'UNSPECIFIED' ) ;
#20094 = DIRECTION ( 'NONE',  ( 0.005235963827121951387, -0.9999862922474492821, -7.400535959139851804E-19 ) ) ;
#20095 = ORIENTED_EDGE ( 'NONE', *, *, #9060, .F. ) ;
#20096 = DIRECTION ( 'NONE',  ( 0.000000000000000000, 0.000000000000000000, -1.000000000000000000 ) ) ;
#20097 = UNCERTAINTY_MEASURE_WITH_UNIT (LENGTH_MEASURE( 1.000000000000000082E-05 ), #2396, 'distance_accuracy_value', 'NONE');
#20098 = EDGE_CURVE ( 'NONE', #20342, #13027, #21455, .T. ) ;
#20099 = EDGE_CURVE ( 'NONE', #1307, #11939, #20183, .T. ) ;
#20100 = PRODUCT_DEFINITION_SHAPE ( 'NONE', 'NONE',  #23497 ) ;
#20101 = CC_DESIGN_APPROVAL ( #14233, ( #12504 ) ) ;
#20102 = ORIENTED_EDGE ( 'NONE', *, *, #18634, .F. ) ;
#20103 = ORIENTED_EDGE ( 'NONE', *, *, #2300, .T. ) ;
#20104 = LINE ( 'NONE', #256, #7707 ) ;
#20105 = DIRECTION ( 'NONE',  ( -6.662111519016958720E-09, 1.000000000000000000, -2.523234146875356491E-15 ) ) ;
#20106 = APPROVAL_PERSON_ORGANIZATION ( #7773, #3940, #4088 ) ;
#20107 = ORIENTED_EDGE ( 'NONE', *, *, #9478, .T. ) ;
#20108 = AXIS2_PLACEMENT_3D ( 'NONE', #17582, #22664, #6409 ) ;
#20109 = CYLINDRICAL_SURFACE ( 'NONE', #882, 2.999999999999999556 ) ;
#20110 = ORIENTED_EDGE ( 'NONE', *, *, #7767, .T. ) ;
#20111 = LINE ( 'NONE', #14999, #18114 ) ;
#20112 = SECURITY_CLASSIFICATION_LEVEL ( 'unclassified' ) ;
#20113 = DIRECTION ( 'NONE',  ( -3.099353312215989243E-62, -1.872670541876879671E-92, 1.000000000000000000 ) ) ;
#20114 = VECTOR ( 'NONE', #19492, 1000.000000000000227 ) ;
#20115 =( LENGTH_UNIT ( ) NAMED_UNIT ( * ) SI_UNIT ( .MILLI., .METRE. ) );
#20116 = CIRCLE ( 'NONE', #3434, 2.750000000000001332 ) ;
#20117 = DIRECTION ( 'NONE',  ( 5.500811659918190397E-13, 0.000000000000000000, -1.000000000000000000 ) ) ;
#20118 = DIRECTION ( 'NONE',  ( -0.9730401042858035643, 0.2306359803922028717, -2.804983810440358308E-16 ) ) ;
#20119 = ADVANCED_FACE ( 'NONE', ( #17556 ), #3285, .T. ) ;
#20120 = DATE_AND_TIME ( #4202, #14814 ) ;
#20121 = APPROVAL_PERSON_ORGANIZATION ( #16505, #20557, #10963 ) ;
#20122 = APPROVAL_PERSON_ORGANIZATION ( #13229, #17941, #16895 ) ;
#20123 = CARTESIAN_POINT ( 'NONE',  ( 52.26033179423370001, -7.535689554643851373, 15.50000000000019895 ) ) ;
#20124 = CARTESIAN_POINT ( 'NONE',  ( 37.01481097301073930, 22.79827665208023291, -11.00000000000049560 ) ) ;
#20125 = CC_DESIGN_PERSON_AND_ORGANIZATION_ASSIGNMENT ( #9366, #10703, ( #1599 ) ) ;
#20126 = CARTESIAN_POINT ( 'NONE',  ( -60.02994014102380049, 8.478793778983318319, 5.000000000000000000 ) ) ;
#20127 = DIRECTION ( 'NONE',  ( 2.269747459788994803E-13, 2.220446049250330436E-15, 1.000000000000000000 ) ) ;
#20128 = CC_DESIGN_PERSON_AND_ORGANIZATION_ASSIGNMENT ( #11205, #18182, ( #8383 ) ) ;
#20129 = DIRECTION ( 'NONE',  ( -0.8823529412199823119, 0.4705882352125332901, 8.962737959213505425E-15 ) ) ;
#20130 = DIRECTION ( 'NONE',  ( 2.270069654138865127E-15, 1.000000000000000000, -4.574083617919690056E-30 ) ) ;
#20131 = CIRCLE ( 'NONE', #12926, 2.066999999999998394 ) ;
#20132 = EDGE_CURVE ( 'NONE', #3011, #15102, #12345, .T. ) ;
#20134 = VERTEX_POINT ( 'NONE', #17784 ) ;
#20133 = ADVANCED_FACE ( 'NONE', ( #12106 ), #6185, .T. ) ;
#20135 = ADVANCED_BREP_SHAPE_REPRESENTATION ( '', ( #17187, #12739 ), #11247 ) ;
#20136 = EDGE_LOOP ( 'NONE', ( #11253, #923, #2220, #19442, #14382, #12952 ) ) ;
#20137 = CARTESIAN_POINT ( 'NONE',  ( -14.10640258711669937, 21.82649101058139962, 2.499999999999950262 ) ) ;
#20138 = DIRECTION ( 'NONE',  ( -0.2306359803922031215, -0.9730401042858035643, -4.620383928407073520E-16 ) ) ;
#20139 = VERTEX_POINT ( 'NONE', #14568 ) ;
#20140 = CLOSED_SHELL ( 'NONE', ( #22248, #17388, #20702, #11191, #20070, #17512, #6891, #8136, #16811, #3106, #2821, #15569, #8788, #20003, #5365, #15215, #3267, #20553, #16652, #21213, #13622 ) ) ;
#20141 = DIRECTION ( 'NONE',  ( 3.099353312215989243E-62, 0.000000000000000000, -1.000000000000000000 ) ) ;
#20142 = VERTEX_POINT ( 'NONE', #13026 ) ;
#20143 = LOCAL_TIME ( 14, 11, 27.00000000000000000, #13783 ) ;
#20144 = DIRECTION ( 'NONE',  ( 0.000000000000000000, 2.583840697242864839E-16, -1.000000000000000000 ) ) ;
#20145 = APPROVAL_PERSON_ORGANIZATION ( #2783, #22518, #13699 ) ;
#20146 = DATE_TIME_ROLE ( 'classification_date' ) ;
#20147 = LINE ( 'NONE', #3871, #7851 ) ;
#20148 = LOCAL_TIME ( 14, 11, 27.00000000000000000, #12551 ) ;
#20149 = CALENDAR_DATE ( 2026, 31, 10 ) ;
#20150 = CARTESIAN_POINT ( 'NONE',  ( -20.00000000397270128, 22.95208919256889857, -5.499999999995559996 ) ) ;
#20151 = ORIENTED_EDGE ( 'NONE', *, *, #17807, .F. ) ;
#20152 = AXIS2_PLACEMENT_3D ( 'NONE', #13969, #21327, #21443 ) ;
#20153 = ORIENTED_EDGE ( 'NONE', *, *, #626, .F. ) ;
#20154 = EDGE_CURVE ( 'NONE', #20610, #12832, #19826, .T. ) ;
#20155 = DIRECTION ( 'NONE',  ( -0.1982893547227720377, -0.8365715274351381847, -0.5107146084541409614 ) ) ;
#20156 = ORIENTED_EDGE ( 'NONE', *, *, #13585, .F. ) ;
#20157 = DIRECTION ( 'NONE',  ( 1.460302919654610928E-28, 2.469237519705104702E-14, 1.000000000000000000 ) ) ;
#20158 = EDGE_CURVE ( 'NONE', #1899, #23121, #6115, .T. ) ;
#20159 = LOCAL_TIME ( 14, 11, 27.00000000000000000, #9970 ) ;
#20160 = VERTEX_POINT ( 'NONE', #14915 ) ;
#20161 = LOCAL_TIME ( 14, 11, 27.00000000000000000, #14858 ) ;
#20162 = CARTESIAN_POINT ( 'NONE',  ( 35.39446192414881409, 8.932132232240984848, 27.19000000000000128 ) ) ;
#20164 = VECTOR ( 'NONE', #1505, 999.9999999999998863 ) ;
#20163 = DIRECTION ( 'NONE',  ( -0.005235963827108362431, 0.9999862922474493931, 5.936218956694023463E-19 ) ) ;
#20165 = DIRECTION ( 'NONE',  ( 0.000000000000000000, -1.000000000000000000, 9.355573283744330345E-16 ) ) ;
#20166 = ORIENTED_EDGE ( 'NONE', *, *, #10887, .T. ) ;
#20167 = EDGE_CURVE ( 'NONE', #14790, #7803, #14789, .T. ) ;
#20168 = AXIS2_PLACEMENT_3D ( 'NONE', #15822, #23052, #2037 ) ;
#20169 = APPROVAL_ROLE ( '' ) ;
#20170 = EDGE_CURVE ( 'NONE', #12606, #4246, #2199, .T. ) ;
#20171 = CARTESIAN_POINT ( 'NONE',  ( -62.93867965702761325, 12.67062903583649991, 3.427095671567209849E-15 ) ) ;
#20172 = ORGANIZATION ( 'NAUO-ORG23', 'UNSPECIFIED', 'UNSPECIFIED' ) ;
#20173 = ORIENTED_EDGE ( 'NONE', *, *, #7243, .T. ) ;
#20174 = PERSON_AND_ORGANIZATION_ROLE ( 'design_supplier' ) ;
#20175 = ORIENTED_EDGE ( 'NONE', *, *, #4112, .F. ) ;
#20176 = VERTEX_POINT ( 'NONE', #12895 ) ;
#20177 = FACE_BOUND ( 'NONE', #9989, .T. ) ;
#20178 = COORDINATED_UNIVERSAL_TIME_OFFSET ( 0, 0, .AHEAD. ) ;
#20179 = CC_DESIGN_APPROVAL ( #19129, ( #5042 ) ) ;
#20180 = DIRECTION ( 'NONE',  ( 0.000000000000000000, -1.000000000000000000, 0.000000000000000000 ) ) ;
#20181 = CARTESIAN_POINT ( 'NONE',  ( -20.00000000397090005, 22.95208919256900160, 8.000000000004460432 ) ) ;
#20182 = AXIS2_PLACEMENT_3D ( 'NONE', #9121, #3887, #7571 ) ;
#20183 = CIRCLE ( 'NONE', #445, 3.499999999999996891 ) ;
#20184 = AXIS2_PLACEMENT_3D ( 'NONE', #20715, #18598, #13242 ) ;
#20185 = ORGANIZATION ( 'NAUO-ORG32', 'UNSPECIFIED', 'UNSPECIFIED' ) ;
#20186 = CARTESIAN_POINT ( 'NONE',  ( 117.1933702072879981, -12.34113894325840022, 18.89999999999999858 ) ) ;
#20187 = CC_DESIGN_PERSON_AND_ORGANIZATION_ASSIGNMENT ( #12966, #5603, ( #11077 ) ) ;
#20188 = AXIS2_PLACEMENT_3D ( 'NONE', #12613, #5129, #3582 ) ;
#20189 = PERSON_AND_ORGANIZATION ( #11966, #8758 ) ;
#20190 = ORIENTED_EDGE ( 'NONE', *, *, #10947, .F. ) ;
#20191 = CARTESIAN_POINT ( 'NONE',  ( -65.80336369117380002, 8.448563927732790191, -5.000000000000000000 ) ) ;
#20192 = ORIENTED_EDGE ( 'NONE', *, *, #17643, .T. ) ;
#20193 = APPROVAL_PERSON_ORGANIZATION ( #15554, #12859, #15905 ) ;
#20194 = LINE ( 'NONE', #5686, #5228 ) ;
#20195 = CARTESIAN_POINT ( 'NONE',  ( -20.00000000000000000, -20.00000000000000000, 0.000000000000000000 ) ) ;
#20196 = ORIENTED_EDGE ( 'NONE', *, *, #22161, .F. ) ;
#20197 = ORIENTED_EDGE ( 'NONE', *, *, #22651, .F. ) ;
#20198 = CARTESIAN_POINT ( 'NONE',  ( -16.50000000202679828, 1.899127378699200008, -5.499999999996309619 ) ) ;
#20199 = AXIS2_PLACEMENT_3D ( 'NONE', #8462, #11800, #1430 ) ;
#20200 = ORIENTED_EDGE ( 'NONE', *, *, #15746, .T. ) ;
#20201 = AXIS2_PLACEMENT_3D ( 'NONE', #2797, #10059, #22143 ) ;
#20202 = COORDINATED_UNIVERSAL_TIME_OFFSET ( 0, 0, .AHEAD. ) ;
#20203 = EDGE_LOOP ( 'NONE', ( #8897, #13711, #888, #12093 ) ) ;
#20204 = VERTEX_POINT ( 'NONE', #18485 ) ;
#20205 = CARTESIAN_POINT ( 'NONE',  ( -24.50000000000000000, -30.47499999999999787, -19.00000000000000000 ) ) ;
#20206 =( BOUNDED_CURVE ( )  B_SPLINE_CURVE ( 2, ( #8328, #17117, #19367 ),
 .UNSPECIFIED., .F., .F. ) 
 B_SPLINE_CURVE_WITH_KNOTS ( ( 3, 3 ),
 ( 0.000000000000000000, 0.2336872276155859962 ),
 .UNSPECIFIED. ) 
 CURVE ( )  GEOMETRIC_REPRESENTATION_ITEM ( )  RATIONAL_B_SPLINE_CURVE ( ( 1.000000000000000000, 1.154700538379259900, 1.000000000000000000 ) ) 
 REPRESENTATION_ITEM ( '' )  );
#20207 = LINE ( 'NONE', #123, #17649 ) ;
#20208 = PERSON_AND_ORGANIZATION ( #11966, #8758 ) ;
#20209 = PLANE ( 'NONE',  #233 ) ;
#20210 = VECTOR ( 'NONE', #1455, 1000.000000000000227 ) ;
#20211 = EDGE_CURVE ( 'NONE', #8431, #547, #12998, .T. ) ;
#20212 = CARTESIAN_POINT ( 'NONE',  ( 52.26033179423370001, -7.535689554643851373, 10.50000000000019895 ) ) ;
#20213 = AXIS2_PLACEMENT_3D ( 'NONE', #3559, #14358, #2000 ) ;
#20214 = APPROVAL_PERSON_ORGANIZATION ( #154, #2538, #23197 ) ;
#20215 = AXIS2_PLACEMENT_3D ( 'NONE', #14290, #12863, #16532 ) ;
#20216 = ORIENTED_EDGE ( 'NONE', *, *, #17059, .T. ) ;
#20217 = CARTESIAN_POINT ( 'NONE',  ( 34.89491389100820129, 23.30074776265919922, 13.00000000000000000 ) ) ;
#20218 = APPROVAL_DATE_TIME ( #14634, #8156 ) ;
#20219 = AXIS2_PLACEMENT_3D ( 'NONE', #17620, #11946, #8347 ) ;
#20220 = ORIENTED_EDGE ( 'NONE', *, *, #15706, .F. ) ;
#20221 = DIRECTION ( 'NONE',  ( 0.000000000000000000, 0.000000000000000000, -1.000000000000000000 ) ) ;
#20222 = CARTESIAN_POINT ( 'NONE',  ( 34.89491389100810181, 23.30074776265909975, -13.00000000000049916 ) ) ;
#20223 = PLANE ( 'NONE',  #7853 ) ;
#20224 = DIRECTION ( 'NONE',  ( 0.000000000000000000, 0.000000000000000000, -1.000000000000000000 ) ) ;
#20225 = DIRECTION ( 'NONE',  ( 1.159535895544890222E-14, 2.167612681253619929E-15, 1.000000000000000000 ) ) ;
#20226 = ORIENTED_EDGE ( 'NONE', *, *, #5076, .T. ) ;
#20227 = VECTOR ( 'NONE', #6672, 1000.000000000000227 ) ;
#20228 = CARTESIAN_POINT ( 'NONE',  ( 34.17143381353265852, 8.269326149122052882, 8.819913685435246009 ) ) ;
#20229 = CC_DESIGN_APPROVAL ( #2233, ( #6978 ) ) ;
#20230 = ORIENTED_EDGE ( 'NONE', *, *, #19162, .T. ) ;
#20231 = ORIENTED_EDGE ( 'NONE', *, *, #1683, .F. ) ;
#20232 = DIRECTION ( 'NONE',  ( 0.2306359803922080343, 0.9730401042858022320, -5.076717492620541185E-14 ) ) ;
#20233 = CARTESIAN_POINT ( 'NONE',  ( 0.07198767335899446118, 20.91792688872588357, -7.334015174596127755E-15 ) ) ;
#20234 = VERTEX_POINT ( 'NONE', #7333 ) ;
#20235 = CIRCLE ( 'NONE', #9638, 4.250000000000001776 ) ;
#20236 = AXIS2_PLACEMENT_3D ( 'NONE', #17375, #5013, #10142 ) ;
#20237 = CARTESIAN_POINT ( 'NONE',  ( -67.06978017061331343, -25.35162245663349978, -2.500000000000000000 ) ) ;
#20238 = EDGE_CURVE ( 'NONE', #13084, #5502, #22085, .T. ) ;
#20239 = ORIENTED_EDGE ( 'NONE', *, *, #11158, .T. ) ;
#20240 = VECTOR ( 'NONE', #7576, 1000.000000000000000 ) ;
#20241 = DIRECTION ( 'NONE',  ( -6.123230199561449365E-17, -4.868008300101910084E-15, -1.000000000000000000 ) ) ;
#20242 = APPROVAL_ROLE ( '' ) ;
#20243 = CARTESIAN_POINT ( 'NONE',  ( 35.59419854219520118, 9.774809681453540122, 26.30000000000000071 ) ) ;
#20244 = CC_DESIGN_DATE_AND_TIME_ASSIGNMENT ( #8649, #13872, ( #8779 ) ) ;
#20245 =( NAMED_UNIT ( * ) SI_UNIT ( $, .STERADIAN. ) SOLID_ANGLE_UNIT ( ) );
#20246 = CIRCLE ( 'NONE', #12241, 2.380000000000002114 ) ;
#20247 = CARTESIAN_POINT ( 'NONE',  ( 35.59419854219520118, 9.774809681453550780, 26.88000000000000256 ) ) ;
#20248 = ADVANCED_FACE ( 'NONE', ( #9455 ), #21674, .T. ) ;
#20249 = ADVANCED_FACE ( 'NONE', ( #16673 ), #12785, .T. ) ;
#20250 = CYLINDRICAL_SURFACE ( 'NONE', #19264, 2.499999999999998668 ) ;
#20251 = APPROVAL_STATUS ( 'not_yet_approved' ) ;
#20252 = AXIS2_PLACEMENT_3D ( 'NONE', #10431, #6733, #13965 ) ;
#20253 = PLANE ( 'NONE',  #19123 ) ;
#20254 = CARTESIAN_POINT ( 'NONE',  ( -29.94170640616770029, 6.343313258985340042, -3.750000000000000000 ) ) ;
#20255 = CYLINDRICAL_SURFACE ( 'NONE', #14254, 2.750000000000000888 ) ;
#20256 = CARTESIAN_POINT ( 'NONE',  ( -19.49999999982360066, -0.1021026942259809916, -5.000000000000000000 ) ) ;
#20257 = DIRECTION ( 'NONE',  ( -1.000000000000000000, -9.259491321837100239E-11, 2.269596547736281384E-13 ) ) ;
#20258 = DIRECTION ( 'NONE',  ( 0.9730401042858036753, -0.2306359803922031493, 2.740969466505752002E-16 ) ) ;
#20259 = ORIENTED_EDGE ( 'NONE', *, *, #17317, .F. ) ;
#20260 = EDGE_LOOP ( 'NONE', ( #4895, #13504, #7698, #14542 ) ) ;
#20261 = DIRECTION ( 'NONE',  ( 0.9730401042858036753, -0.2306359803922031493, 2.740969466505752002E-16 ) ) ;
#20262 = PLANE ( 'NONE',  #1515 ) ;
#20263 = ORIENTED_EDGE ( 'NONE', *, *, #23038, .F. ) ;
#20264 = DIRECTION ( 'NONE',  ( 0.8846153846154060085, -0.4663213712685030377, 0.000000000000000000 ) ) ;
#20265 = ADVANCED_FACE ( 'NONE', ( #3637 ), #8838, .F. ) ;
#20266 = EDGE_LOOP ( 'NONE', ( #13295, #19090 ) ) ;
#20267 = DIRECTION ( 'NONE',  ( -0.005235963827108362431, 0.9999862922474493931, 5.936218956694023463E-19 ) ) ;
#20268 = PERSON_AND_ORGANIZATION ( #11966, #8758 ) ;
#20269 = AXIS2_PLACEMENT_3D ( 'NONE', #17578, #22906, #1511 ) ;
#20270 = DIRECTION ( 'NONE',  ( 0.2306359803922028717, 0.9730401042858035643, -5.065637133954654909E-15 ) ) ;
#20271 = CC_DESIGN_PERSON_AND_ORGANIZATION_ASSIGNMENT ( #2202, #13030, ( #5427 ) ) ;
#20272 = APPROVAL ( #20513, 'UNSPECIFIED' ) ;
#20273 = DIRECTION ( 'NONE',  ( 0.7071067811865475727, 0.000000000000000000, -0.7071067811865474617 ) ) ;
#20274 = CARTESIAN_POINT ( 'NONE',  ( -1.437248611304650980, 16.42796209631955051, -7.586732966291266084E-17 ) ) ;
#20275 = ADVANCED_FACE ( 'NONE', ( #5887 ), #4104, .T. ) ;
#20276 = ADVANCED_FACE ( 'NONE', ( #7209, #5421, #5766, #12679 ), #9222, .F. ) ;
#20277 = EDGE_LOOP ( 'NONE', ( #13837, #14566, #4533, #21574 ) ) ;
#20278 = CC_DESIGN_PERSON_AND_ORGANIZATION_ASSIGNMENT ( #2878, #3108, ( #21633 ) ) ;
#20279 = DIRECTION ( 'NONE',  ( -0.02168293463503252055, 0.9997648975362223300, -2.428612866367530721E-15 ) ) ;
#20280 = EDGE_LOOP ( 'NONE', ( #10584, #9604, #2738, #7410 ) ) ;
#20281 = SPHERICAL_SURFACE ( 'NONE', #5583, 15.25000000000000000 ) ;
#20282 = CARTESIAN_POINT ( 'NONE',  ( -62.91249983789198552, 7.670697574599230073, 2.108981951733699973E-15 ) ) ;
#20283 = ORIENTED_EDGE ( 'NONE', *, *, #20431, .T. ) ;
#20284 = FACE_OUTER_BOUND ( 'NONE', #14715, .T. ) ;
#20285 = DIRECTION ( 'NONE',  ( -0.6880432561069586006, 0.1630842657209347069, -0.7071067811865459074 ) ) ;
#20286 = DIRECTION ( 'NONE',  ( -0.9730401042858036753, 0.2306359803922028995, 5.959266323858677443E-17 ) ) ;
#20287 = VERTEX_POINT ( 'NONE', #21911 ) ;
#20288 = SECURITY_CLASSIFICATION_LEVEL ( 'unclassified' ) ;
#20289 = ORIENTED_EDGE ( 'NONE', *, *, #3720, .F. ) ;
#20290 = PERSON_AND_ORGANIZATION ( #11966, #8758 ) ;
#20291 = LINE ( 'NONE', #14264, #5768 ) ;
#20292 = EDGE_CURVE ( 'NONE', #6032, #6621, #18373, .T. ) ;
#20293 = VERTEX_POINT ( 'NONE', #19915 ) ;
#20294 = ORIENTED_EDGE ( 'NONE', *, *, #21093, .F. ) ;
#20295 = CARTESIAN_POINT ( 'NONE',  ( 37.56481403710121469, 24.44795204016919854, 14.00000000000001066 ) ) ;
#20296 = CALENDAR_DATE ( 2026, 31, 10 ) ;
#20297 = EDGE_CURVE ( 'NONE', #13601, #17440, #9334, .T. ) ;
#20298 = CIRCLE ( 'NONE', #21057, 2.999999999999999556 ) ;
#20299 = APPROVAL_ROLE ( '' ) ;
#20300 = LINE ( 'NONE', #13177, #9293 ) ;
#20301 = EDGE_CURVE ( 'NONE', #20234, #14214, #1235, .T. ) ;
#20302 = EDGE_CURVE ( 'NONE', #2200, #8857, #4657, .T. ) ;
#20303 = DIRECTION ( 'NONE',  ( -0.9730401042858035643, 0.2306359803922028717, 5.958148513035547083E-17 ) ) ;
#20304 = COORDINATED_UNIVERSAL_TIME_OFFSET ( 0, 0, .AHEAD. ) ;
#20305 = PRODUCT_DEFINITION_SHAPE ( 'NONE', 'NONE',  #10554 ) ;
#20306 = ORIENTED_EDGE ( 'NONE', *, *, #22952, .F. ) ;
#20307 = CARTESIAN_POINT ( 'NONE',  ( -27.00000000000000000, -27.34999999999999787, 2.500000000000000000 ) ) ;
#20308 = ORIENTED_EDGE ( 'NONE', *, *, #10858, .T. ) ;
#20309 = DIRECTION ( 'NONE',  ( -0.9730401042858022320, 0.2306359803922080343, 5.959266323858941219E-17 ) ) ;
#20310 = DIRECTION ( 'NONE',  ( 3.099353312215989243E-62, -9.554441540188157279E-93, -1.000000000000000000 ) ) ;
#20311 = CARTESIAN_POINT ( 'NONE',  ( -3.458317987535627580, 19.03127855354509990, -7.999999999999998224 ) ) ;
#20312 = ORIENTED_EDGE ( 'NONE', *, *, #13414, .T. ) ;
#20313 = ORIENTED_EDGE ( 'NONE', *, *, #7108, .F. ) ;
#20314 = CARTESIAN_POINT ( 'NONE',  ( 58.25686728443099582, 17.76335315678740301, -13.00000000000049916 ) ) ;
#20315 = VERTEX_POINT ( 'NONE', #643 ) ;
#20316 = CALENDAR_DATE ( 2026, 31, 10 ) ;
#20317 = ORIENTED_EDGE ( 'NONE', *, *, #20167, .F. ) ;
#20318 = ORIENTED_EDGE ( 'NONE', *, *, #14015, .T. ) ;
#20319 = CARTESIAN_POINT ( 'NONE',  ( -25.49858938551139786, -0.2322002804899460093, -3.750000000000000000 ) ) ;
#20320 = CARTESIAN_POINT ( 'NONE',  ( -22.52506282043239594, 26.45208917575140006, -7.999999999994998667 ) ) ;
#20321 = PERSON_AND_ORGANIZATION_ROLE ( 'design_supplier' ) ;
#20322 = DIRECTION ( 'NONE',  ( -1.000000000000000000, 0.000000000000000000, 0.000000000000000000 ) ) ;
#20323 = CARTESIAN_POINT ( 'NONE',  ( 44.61084671068384466, 26.13635165663675153, -18.00000000000029843 ) ) ;
#20324 = EDGE_CURVE ( 'NONE', #4600, #11347, #22606, .T. ) ;
#20325 = ORIENTED_EDGE ( 'NONE', *, *, #5431, .F. ) ;
#20326 = AXIS2_PLACEMENT_3D ( 'NONE', #17816, #19244, #8679 ) ;
#20327 = DIRECTION ( 'NONE',  ( 0.9730401042858035643, -0.2306359803922028717, -5.432877459303547053E-17 ) ) ;
#20328 = PERSON_AND_ORGANIZATION ( #11966, #8758 ) ;
#20329 = ORIENTED_EDGE ( 'NONE', *, *, #19520, .T. ) ;
#20330 = LINE ( 'NONE', #4059, #751 ) ;
#20331 = CARTESIAN_POINT ( 'NONE',  ( -69.82862846239019916, -8.365734848149529057, -7.200000000000000178 ) ) ;
#20332 = ADVANCED_FACE ( 'NONE', ( #19074 ), #4460, .T. ) ;
#20333 = DIRECTION ( 'NONE',  ( 0.9730401042858035643, -0.2306359803922028717, -5.959266323858667582E-17 ) ) ;
#20334 =( BOUNDED_CURVE ( )  B_SPLINE_CURVE ( 2, ( #18476, #16550, #12883 ),
 .UNSPECIFIED., .F., .F. ) 
 B_SPLINE_CURVE_WITH_KNOTS ( ( 3, 3 ),
 ( 0.000000000000000000, 0.1752654207116860208 ),
 .UNSPECIFIED. ) 
 CURVE ( )  GEOMETRIC_REPRESENTATION_ITEM ( )  RATIONAL_B_SPLINE_CURVE ( ( 1.000000000000000000, 1.154700538379249908, 1.000000000000000000 ) ) 
 REPRESENTATION_ITEM ( '' )  );
#20335 = DIRECTION ( 'NONE',  ( -1.000000000000000000, -6.662111140531837817E-09, 1.144917494144693313E-14 ) ) ;
#20336 = ORIENTED_EDGE ( 'NONE', *, *, #17254, .T. ) ;
#20337 = DIRECTION ( 'NONE',  ( -0.9730401042858023430, 0.2306359803922080620, 5.959266323858944916E-17 ) ) ;
#20338 = DESIGN_CONTEXT ( 'detailed design', #20351, 'design' ) ;
#20339 = APPROVAL_DATE_TIME ( #13338, #8675 ) ;
#20340 = CIRCLE ( 'NONE', #10121, 4.250000000000000000 ) ;
#20341 = VERTEX_POINT ( 'NONE', #20838 ) ;
#20342 = VERTEX_POINT ( 'NONE', #9709 ) ;
#20343 = DIRECTION ( 'NONE',  ( -0.9730401042858037863, 0.2306359803922024276, 5.958148513035967398E-17 ) ) ;
#20344 = DIRECTION ( 'NONE',  ( 0.9730401042858036753, -0.2306359803922028995, -5.432877459303547669E-17 ) ) ;
#20345 = ORIENTED_EDGE ( 'NONE', *, *, #9988, .F. ) ;
#20346 = COORDINATED_UNIVERSAL_TIME_OFFSET ( 0, 0, .AHEAD. ) ;
#20347 = DIRECTION ( 'NONE',  ( -0.2306359803922080620, -0.9730401042858023430, 4.455014470410797513E-15 ) ) ;
#20348 = DIRECTION ( 'NONE',  ( -3.099353312215989243E-62, 1.534091707905539548E-92, 1.000000000000000000 ) ) ;
#20349 = DATE_AND_TIME ( #18464, #21362 ) ;
#20350 = CARTESIAN_POINT ( 'NONE',  ( -29.01753512594849838, 6.974156885510950588, 5.000000000000000000 ) ) ;
#20351 = APPLICATION_CONTEXT ( 'configuration controlled 3d designs of mechanical parts and assemblies' ) ;
#20352 = CARTESIAN_POINT ( 'NONE',  ( -26.68810977484059777, -6.639828994528159889, -2.500000000000090150 ) ) ;
#20353 = CARTESIAN_POINT ( 'NONE',  ( -65.62876257020761273, -24.89748912807110059, -5.000000000000000000 ) ) ;
#20354 = PERSON_AND_ORGANIZATION_ROLE ( 'design_owner' ) ;
#20355 = CONICAL_SURFACE ( 'NONE', #10139, 2.283500000000000529, 0.7853981633974469467 ) ;
#20356 = AXIS2_PLACEMENT_3D ( 'NONE', #7118, #5661, #13050 ) ;
#20357 = AXIS2_PLACEMENT_3D ( 'NONE', #11826, #19631, #3356 ) ;
#20358 = FACE_OUTER_BOUND ( 'NONE', #13076, .T. ) ;
#20359 = DIRECTION ( 'NONE',  ( 0.9730401042858036753, -0.2306359803922028995, -5.432877459303547669E-17 ) ) ;
#20360 = EDGE_CURVE ( 'NONE', #12832, #6522, #17566, .T. ) ;
#20361 = DIRECTION ( 'NONE',  ( 3.330999558967088958E-36, 2.805478249480050404E-20, 1.000000000000000000 ) ) ;
#20362 = EDGE_CURVE ( 'NONE', #2081, #20661, #2800, .T. ) ;
#20363 = LINE ( 'NONE', #20828, #7971 ) ;
#20364 = CYLINDRICAL_SURFACE ( 'NONE', #14167, 6.000000000000109246 ) ;
#20365 = CARTESIAN_POINT ( 'NONE',  ( 33.87576285740830428, 21.16892588828849853, 13.00000000000000000 ) ) ;
#20366 = ORIENTED_EDGE ( 'NONE', *, *, #8628, .F. ) ;
#20367 = ORIENTED_EDGE ( 'NONE', *, *, #17934, .T. ) ;
#20368 = LINE ( 'NONE', #4348, #839 ) ;
#20369 = DIRECTION ( 'NONE',  ( -6.662111938308250854E-09, 1.000000000000000000, -2.220444537119161047E-15 ) ) ;
#20370 = AXIS2_PLACEMENT_3D ( 'NONE', #1803, #2050, #19751 ) ;
#20371 = ORIENTED_EDGE ( 'NONE', *, *, #16368, .F. ) ;
#20372 = EDGE_CURVE ( 'NONE', #2287, #3272, #22484, .T. ) ;
#20373 = EDGE_CURVE ( 'NONE', #16709, #20610, #22374, .T. ) ;
#20374 = DIRECTION ( 'NONE',  ( -0.04564792618500997101, -0.9989575901083128651, 2.775557561562890562E-15 ) ) ;
#20375 = ORIENTED_EDGE ( 'NONE', *, *, #23171, .F. ) ;
#20376 = DIRECTION ( 'NONE',  ( -0.2306359803922080343, -0.9730401042858022320, -1.780177465867830349E-15 ) ) ;
#20377 = VECTOR ( 'NONE', #2367, 1000.000000000000227 ) ;
#20378 = APPROVAL_STATUS ( 'not_yet_approved' ) ;
#20379 = CARTESIAN_POINT ( 'NONE',  ( 31.45181451370271475, 16.90945435098595340, 21.49999999999999289 ) ) ;
#20380 = CIRCLE ( 'NONE', #7124, 2.500000000000000000 ) ;
#20381 = CYLINDRICAL_SURFACE ( 'NONE', #4094, 3.499999999999998668 ) ;
#20382 = ORIENTED_EDGE ( 'NONE', *, *, #19445, .T. ) ;
#20383 = VECTOR ( 'NONE', #6912, 1000.000000000000000 ) ;
#20384 = DIRECTION ( 'NONE',  ( -1.000000000000000000, 2.775557561562891351E-15, 0.000000000000000000 ) ) ;
#20385 = VERTEX_POINT ( 'NONE', #753 ) ;
#20386 = CARTESIAN_POINT ( 'NONE',  ( 35.59419854219520118, 9.774809681453270116, -29.25000000000050093 ) ) ;
#20387 = CIRCLE ( 'NONE', #21513, 2.066999999999997506 ) ;
#20388 = EDGE_CURVE ( 'NONE', #1609, #4918, #8094, .T. ) ;
#20389 = VECTOR ( 'NONE', #7246, 1000.000000000000000 ) ;
#20390 = CARTESIAN_POINT ( 'NONE',  ( -20.00000000397270128, 22.95208919256889857, -4.999999999995559996 ) ) ;
#20391 = CIRCLE ( 'NONE', #10179, 2.499999999999998668 ) ;
#20392 = VERTEX_POINT ( 'NONE', #15495 ) ;
#20393 = CARTESIAN_POINT ( 'NONE',  ( -60.06514239919540188, -6.814592325618320068, 3.000000000000100364 ) ) ;
#20394 = FACE_BOUND ( 'NONE', #10769, .T. ) ;
#20395 = CARTESIAN_POINT ( 'NONE',  ( -69.88753305544580030, 2.884110939634079607, 3.000000000000100364 ) ) ;
#20396 = EDGE_LOOP ( 'NONE', ( #20793, #4924, #4698, #19587 ) ) ;
#20397 = APPROVAL ( #1585, 'UNSPECIFIED' ) ;
#20398 = APPROVAL_DATE_TIME ( #4127, #3685 ) ;
#20399 = CC_DESIGN_DATE_AND_TIME_ASSIGNMENT ( #13687, #4538, ( #13725 ) ) ;
#20400 = CARTESIAN_POINT ( 'NONE',  ( 37.01481097301073930, 22.79827665208023291, -11.00000000000049560 ) ) ;
#20401 = VECTOR ( 'NONE', #17786, 999.9999999999998863 ) ;
#20402 = ORIENTED_EDGE ( 'NONE', *, *, #4906, .F. ) ;
#20403 = ADVANCED_FACE ( 'NONE', ( #18949, #9937 ), #8026, .F. ) ;
#20404 = EDGE_CURVE ( 'NONE', #5266, #10552, #6944, .T. ) ;
#20405 = APPROVAL_STATUS ( 'not_yet_approved' ) ;
#20406 = ORIENTED_EDGE ( 'NONE', *, *, #9828, .T. ) ;
#20407 = ORIENTED_EDGE ( 'NONE', *, *, #19537, .T. ) ;
#20408 = DIRECTION ( 'NONE',  ( 0.000000000000000000, -1.000000000000000000, 0.000000000000000000 ) ) ;
#20409 = AXIS2_PLACEMENT_3D ( 'NONE', #17228, #17577, #4625 ) ;
#20410 = APPROVAL_DATE_TIME ( #16846, #10427 ) ;
#20411 = EDGE_CURVE ( 'NONE', #17785, #3517, #11618, .T. ) ;
#20412 = ITEM_DEFINED_TRANSFORMATION ( 'NONE', 'NONE', #4959,  #12739 ) ;
#20413 = AXIS2_PLACEMENT_3D ( 'NONE', #2268, #18679, #2400 ) ;
#20414 = FACE_OUTER_BOUND ( 'NONE', #21338, .T. ) ;
#20415 = PERSON ( 'NAUO-PER41', 'UNSPECIFIED', 'UNSPECIFIED', ('UNSPECIFIED'), ('UNSPECIFIED'), ('UNSPECIFIED') ) ;
#20416 = CARTESIAN_POINT ( 'NONE',  ( -20.00000000000000000, -20.00000000000000000, 0.000000000000000000 ) ) ;
#20417 = APPROVAL_STATUS ( 'not_yet_approved' ) ;
#20418 = EDGE_CURVE ( 'NONE', #22408, #10449, #18845, .T. ) ;
#20419 = ORIENTED_EDGE ( 'NONE', *, *, #7093, .T. ) ;
#20420 = CARTESIAN_POINT ( 'NONE',  ( -17.47493720815199936, 28.95208920939580111, 5.500000000004419576 ) ) ;
#20421 = EDGE_LOOP ( 'NONE', ( #4488, #14948, #261, #1893 ) ) ;
#20422 = CARTESIAN_POINT ( 'NONE',  ( -29.01753512594849838, 6.974156885510950588, 3.750000000000000000 ) ) ;
#20424 = CIRCLE ( 'NONE', #6013, 4.099999999999999645 ) ;
#20423 = CARTESIAN_POINT ( 'NONE',  ( -59.07950864401303193, -25.30978511045550050, -3.660254037844393071 ) ) ;
#20425 = DIRECTION ( 'NONE',  ( 0.2306359803922080898, 0.9730401042858024541, -2.572202231434325988E-16 ) ) ;
#20426 = ORIENTED_EDGE ( 'NONE', *, *, #19445, .F. ) ;
#20427 = ORIENTED_EDGE ( 'NONE', *, *, #21421, .T. ) ;
#20428 = DIRECTION ( 'NONE',  ( 2.982858504577314686E-17, -2.441916418604790135E-15, -1.000000000000000000 ) ) ;
#20429 = ORIENTED_EDGE ( 'NONE', *, *, #1837, .F. ) ;
#20430 = EDGE_CURVE ( 'NONE', #19075, #13601, #20678, .T. ) ;
#20431 = EDGE_CURVE ( 'NONE', #4956, #15418, #10748, .T. ) ;
#20432 = PERSON_AND_ORGANIZATION ( #11966, #8758 ) ;
#20433 = PERSON ( 'NAUO-PER5', 'UNSPECIFIED', 'UNSPECIFIED', ('UNSPECIFIED'), ('UNSPECIFIED'), ('UNSPECIFIED') ) ;
#20434 = EDGE_LOOP ( 'NONE', ( #12363, #18193, #12441, #22542 ) ) ;
#20435 = ORIENTED_EDGE ( 'NONE', *, *, #14997, .T. ) ;
#20436 = CARTESIAN_POINT ( 'NONE',  ( -26.26776695296636888, -31.09999999999999432, 20.76776695296636888 ) ) ;
#20437 = CARTESIAN_POINT ( 'NONE',  ( 5.750000000000139444, -20.33108891324529921, -2.500000000000000000 ) ) ;
#20438 = PERSON_AND_ORGANIZATION_ROLE ( 'design_supplier' ) ;
#20439 = PLANE ( 'NONE',  #12394 ) ;
#20440 = LINE ( 'NONE', #9050, #19746 ) ;
#20441 = EDGE_LOOP ( 'NONE', ( #20263, #9128, #18916, #19029 ) ) ;
#20442 = DIRECTION ( 'NONE',  ( 0.000000000000000000, 0.000000000000000000, -1.000000000000000000 ) ) ;
#20443 = PERSON_AND_ORGANIZATION ( #11966, #8758 ) ;
#20444 = EDGE_CURVE ( 'NONE', #5198, #9054, #537, .T. ) ;
#20445 = ORIENTED_EDGE ( 'NONE', *, *, #2743, .T. ) ;
#20446 = DIRECTION ( 'NONE',  ( -1.000000000000000000, 0.000000000000000000, 0.000000000000000000 ) ) ;
#20447 = CIRCLE ( 'NONE', #2289, 2.066999999999999726 ) ;
#20448 = DIRECTION ( 'NONE',  ( 0.000000000000000000, 0.000000000000000000, -1.000000000000000000 ) ) ;
#20449 = ORIENTED_EDGE ( 'NONE', *, *, #16305, .T. ) ;
#20450 = DIRECTION ( 'NONE',  ( -6.123237831918399306E-17, 1.569224110909209817E-30, 1.000000000000000000 ) ) ;
#20451 = LINE ( 'NONE', #2409, #1603 ) ;
#20452 = VERTEX_POINT ( 'NONE', #2319 ) ;
#20453 = DIRECTION ( 'NONE',  ( -0.2306359803921919083, -0.9730401042858062288, -1.333568672157176260E-13 ) ) ;
#20454 = EDGE_CURVE ( 'NONE', #5242, #19229, #9581, .T. ) ;
#20455 = MECHANICAL_CONTEXT ( 'NONE', #18393, 'mechanical' ) ;
#20457 = ADVANCED_FACE ( 'NONE', ( #13249 ), #20486, .T. ) ;
#20456 = ORIENTED_EDGE ( 'NONE', *, *, #19017, .T. ) ;
#20458 = ORIENTED_EDGE ( 'NONE', *, *, #1239, .F. ) ;
#20459 = CARTESIAN_POINT ( 'NONE',  ( -20.00000000000000000, -20.00000000000000000, -5.499999999995469402 ) ) ;
#20460 = CYLINDRICAL_SURFACE ( 'NONE', #13636, 2.499999999999999112 ) ;
#20461 = ORIENTED_EDGE ( 'NONE', *, *, #22749, .F. ) ;
#20462 = PERSON_AND_ORGANIZATION ( #11966, #8758 ) ;
#20463 = CARTESIAN_POINT ( 'NONE',  ( -25.44812980900369936, 25.46511081327010118, 2.499999999999940048 ) ) ;
#20464 = DIRECTION ( 'NONE',  ( -1.000000000000000000, 2.270069654138870255E-15, 0.000000000000000000 ) ) ;
#20465 = LOCAL_TIME ( 14, 11, 27.00000000000000000, #10706 ) ;
#20466 = AXIS2_PLACEMENT_3D ( 'NONE', #1700, #16300, #20105 ) ;
#20467 = DIRECTION ( 'NONE',  ( 2.982858504489129897E-17, -2.441916418604790135E-15, -1.000000000000000000 ) ) ;
#20468 = LINE ( 'NONE', #9316, #17199 ) ;
#20469 = DIRECTION ( 'NONE',  ( 0.000000000000000000, 0.000000000000000000, -1.000000000000000000 ) ) ;
#20470 = APPROVAL_ROLE ( '' ) ;
#20471 = DIRECTION ( 'NONE',  ( 1.000000000000000000, 6.123237831918438750E-17, -1.555753819465284865E-62 ) ) ;
#20472 = CARTESIAN_POINT ( 'NONE',  ( -3.499952022866070767, -0.01832587339492825623, 2.500000000000090594 ) ) ;
#20473 = CC_DESIGN_PERSON_AND_ORGANIZATION_ASSIGNMENT ( #8946, #19979, ( #796 ) ) ;
#20474 = CARTESIAN_POINT ( 'NONE',  ( -20.00000000397469790, 22.95208919256889857, -8.499999999995548450 ) ) ;
#20475 = DIRECTION ( 'NONE',  ( 0.9999862922474493931, 0.005235963827101436548, -1.187304881134279227E-16 ) ) ;
#20476 = VECTOR ( 'NONE', #23320, 999.9999999999998863 ) ;
#20477 = FACE_OUTER_BOUND ( 'NONE', #18998, .T. ) ;
#20478 = AXIS2_PLACEMENT_3D ( 'NONE', #8195, #15425, #15676 ) ;
#20479 = PLANE ( 'NONE',  #14134 ) ;
#20480 = ORIENTED_EDGE ( 'NONE', *, *, #9799, .F. ) ;
#20481 = ORIENTED_EDGE ( 'NONE', *, *, #18353, .F. ) ;
#20482 = CARTESIAN_POINT ( 'NONE',  ( 118.4388045014059969, -7.086722380115159758, -19.59999999999999787 ) ) ;
#20483 = DIRECTION ( 'NONE',  ( -5.401314170743249993E-15, -2.304622183485879988E-14, 1.000000000000000000 ) ) ;
#20484 = ORIENTED_EDGE ( 'NONE', *, *, #6445, .T. ) ;
#20485 = VECTOR ( 'NONE', #3946, 1000.000000000000000 ) ;
#20486 = CYLINDRICAL_SURFACE ( 'NONE', #20593, 1.000000000000000000 ) ;
#20487 = ORIENTED_EDGE ( 'NONE', *, *, #20877, .F. ) ;
#20488 = CARTESIAN_POINT ( 'NONE',  ( 36.57467860885130051, 21.71590586959139912, 11.00000000000000000 ) ) ;
#20489 = VECTOR ( 'NONE', #12164, 999.9999999999997726 ) ;
#20490 = PERSON_AND_ORGANIZATION ( #11966, #8758 ) ;
#20491 = CARTESIAN_POINT ( 'NONE',  ( -20.00000000000000000, -20.00000000000000000, 0.000000000000000000 ) ) ;
#20492 = APPLICATION_CONTEXT ( 'configuration controlled 3d designs of mechanical parts and assemblies' ) ;
#20493 = EDGE_CURVE ( 'NONE', #16294, #255, #17521, .T. ) ;
#20494 = PRODUCT_DEFINITION_SHAPE ( 'NONE', 'NONE',  #23484 ) ;
#20495 = SECURITY_CLASSIFICATION ( '', '', #22541 ) ;
#20496 = CALENDAR_DATE ( 2026, 31, 10 ) ;
#20497 = DIRECTION ( 'NONE',  ( -0.9730401042858024541, 0.2306359803922080898, 5.959266323858472832E-17 ) ) ;
#20498 = ORIENTED_EDGE ( 'NONE', *, *, #17781, .T. ) ;
#20499 = CARTESIAN_POINT ( 'NONE',  ( 36.34169561367309598, 12.92845737834459996, -29.25000000000050093 ) ) ;
#20500 = ORIENTED_EDGE ( 'NONE', *, *, #2097, .T. ) ;
#20502 = CONICAL_SURFACE ( 'NONE', #22389, 2.254620000000000513, 0.7853981633974461696 ) ;
#20501 = DIRECTION ( 'NONE',  ( -3.210834492181040124E-17, 2.441916418604790135E-15, 1.000000000000000000 ) ) ;
#20503 = DIRECTION ( 'NONE',  ( 0.2306359803922080343, 0.9730401042858022320, 3.574477303645861237E-15 ) ) ;
#20504 = ORIENTED_EDGE ( 'NONE', *, *, #7027, .T. ) ;
#20505 = CARTESIAN_POINT ( 'NONE',  ( -22.99999999999959854, -19.33065833018789803, 21.49999999999999289 ) ) ;
#20506 = CARTESIAN_POINT ( 'NONE',  ( -19.49999999982519938, -0.1021026942257889925, -5.000000000000000000 ) ) ;
#20507 = VERTEX_POINT ( 'NONE', #8612 ) ;
#20508 = LOCAL_TIME ( 14, 11, 27.00000000000000000, #15575 ) ;
#20509 = PERSON_AND_ORGANIZATION ( #5392, #6542 ) ;
#20510 = CARTESIAN_POINT ( 'NONE',  ( 30.57814311865390167, -3.583136841840119935, -15.00000000000039968 ) ) ;
#20511 = APPROVAL_PERSON_ORGANIZATION ( #21375, #19129, #17349 ) ;
#20512 = ORIENTED_EDGE ( 'NONE', *, *, #12396, .F. ) ;
#20513 = APPROVAL_STATUS ( 'not_yet_approved' ) ;
#20514 = FACE_OUTER_BOUND ( 'NONE', #21849, .T. ) ;
#20515 = EDGE_LOOP ( 'NONE', ( #3385, #20345, #22979, #13816 ) ) ;
#20516 = ORIENTED_EDGE ( 'NONE', *, *, #9544, .F. ) ;
#20517 = ORGANIZATION ( 'NAUO-ORG39', 'UNSPECIFIED', 'UNSPECIFIED' ) ;
#20518 = CYLINDRICAL_SURFACE ( 'NONE', #3137, 2.499999999999999556 ) ;
#20519 = APPROVAL_ROLE ( '' ) ;
#20520 = AXIS2_PLACEMENT_3D ( 'NONE', #9697, #7894, #9807 ) ;
#20521 = EDGE_CURVE ( 'NONE', #7380, #2028, #5052, .T. ) ;
#20522 = APPROVAL_STATUS ( 'not_yet_approved' ) ;
#20523 = CARTESIAN_POINT ( 'NONE',  ( 28.27870060330360147, -2.444761924717900214, -11.00000000000039968 ) ) ;
#20524 = CC_DESIGN_DATE_AND_TIME_ASSIGNMENT ( #1025, #17562, ( #9926 ) ) ;
#20525 = LOCAL_TIME ( 14, 11, 27.00000000000000000, #21476 ) ;
#20526 = LOCAL_TIME ( 14, 11, 27.00000000000000000, #17249 ) ;
#20527 = DIRECTION ( 'NONE',  ( -6.662161563160872600E-09, 1.000000000000000000, -1.982541115402066096E-15 ) ) ;
#20528 = CIRCLE ( 'NONE', #13721, 2.066999999999999726 ) ;
#20529 = ORIENTED_EDGE ( 'NONE', *, *, #16218, .F. ) ;
#20530 = EDGE_CURVE ( 'NONE', #13027, #15043, #1347, .T. ) ;
#20531 = ADVANCED_FACE ( 'NONE', ( #8507 ), #23075, .T. ) ;
#20532 = PERSON_AND_ORGANIZATION ( #11966, #8758 ) ;
#20533 = EDGE_LOOP ( 'NONE', ( #23339, #11322, #5182, #11775, #18618 ) ) ;
#20534 = APPROVAL_PERSON_ORGANIZATION ( #4256, #5292, #4136 ) ;
#20535 = APPLICATION_CONTEXT ( 'configuration controlled 3d designs of mechanical parts and assemblies' ) ;
#20536 = CARTESIAN_POINT ( 'NONE',  ( 43.45766680872284837, 21.27115113520789791, 12.99999999999970157 ) ) ;
#20537 = EDGE_LOOP ( 'NONE', ( #7512, #13835, #3282, #16852 ) ) ;
#20538 = DIRECTION ( 'NONE',  ( 0.000000000000000000, 0.000000000000000000, -1.000000000000000000 ) ) ;
#20539 = PLANE ( 'NONE',  #8517 ) ;
#20540 = SHAPE_REPRESENTATION ( '1602p_c_41', ( #12739 ), #21598 ) ;
#20541 = FACE_OUTER_BOUND ( 'NONE', #16424, .T. ) ;
#20542 = VERTEX_POINT ( 'NONE', #6719 ) ;
#20543 = ORIENTED_EDGE ( 'NONE', *, *, #11031, .T. ) ;
#20544 = CARTESIAN_POINT ( 'NONE',  ( -19.49999999982360066, -0.1021026942259579962, 5.000000000000000000 ) ) ;
#20545 = ORIENTED_EDGE ( 'NONE', *, *, #17355, .F. ) ;
#20546 = PERSON_AND_ORGANIZATION ( #11966, #8758 ) ;
#20547 = LOCAL_TIME ( 14, 11, 27.00000000000000000, #13749 ) ;
#20548 = ORIENTED_EDGE ( 'NONE', *, *, #595, .F. ) ;
#20549 = ORIENTED_EDGE ( 'NONE', *, *, #21862, .T. ) ;
#20550 = CARTESIAN_POINT ( 'NONE',  ( 5.000000000000000000, -23.36217782649100272, 5.000000000000000000 ) ) ;
#20551 = PERSON_AND_ORGANIZATION ( #11966, #8758 ) ;
#20552 = CARTESIAN_POINT ( 'NONE',  ( 35.59419854219520118, 9.774809681453278998, -26.69000000000049866 ) ) ;
#20553 = ADVANCED_FACE ( 'NONE', ( #10417 ), #15736, .F. ) ;
#20554 = CARTESIAN_POINT ( 'NONE',  ( 33.90884364377009774, 10.17428291754599989, -29.25000000000050093 ) ) ;
#20555 = CC_DESIGN_APPROVAL ( #15592, ( #16748 ) ) ;
#20556 = CC_DESIGN_DATE_AND_TIME_ASSIGNMENT ( #10476, #17457, ( #5042 ) ) ;
#20557 = APPROVAL ( #9279, 'UNSPECIFIED' ) ;
#20558 = EDGE_CURVE ( 'NONE', #903, #13085, #6834, .T. ) ;
#20559 = ADVANCED_FACE ( 'NONE', ( #4806 ), #3020, .T. ) ;
#20560 = DIRECTION ( 'NONE',  ( -1.000000000000000000, 0.000000000000000000, 0.000000000000000000 ) ) ;
#20561 = PERSON_AND_ORGANIZATION ( #11966, #8758 ) ;
#20562 = CC_DESIGN_SECURITY_CLASSIFICATION ( #15633, ( #11856 ) ) ;
#20563 = CC_DESIGN_PERSON_AND_ORGANIZATION_ASSIGNMENT ( #20189, #9633, ( #3780 ) ) ;
#20564 = EDGE_LOOP ( 'NONE', ( #17038, #12731, #7789, #10108 ) ) ;
#20565 = CARTESIAN_POINT ( 'NONE',  ( 37.48968750243700043, 22.68571848161329996, 14.15470053837925057 ) ) ;
#20566 = AXIS2_PLACEMENT_3D ( 'NONE', #15343, #17368, #22808 ) ;
#20567 = CARTESIAN_POINT ( 'NONE',  ( 33.27705887009690144, -3.036156860537079893, 13.00000000000019895 ) ) ;
#20568 = ORIENTED_EDGE ( 'NONE', *, *, #10005, .T. ) ;
#20569 = CARTESIAN_POINT ( 'NONE',  ( -20.00000000397360012, 22.95208919256889857, -2.500000000000039968 ) ) ;
#20570 = CIRCLE ( 'NONE', #19056, 3.750000000000000000 ) ;
#20571 = AXIS2_PLACEMENT_3D ( 'NONE', #3170, #10441, #22981 ) ;
#20572 = DIRECTION ( 'NONE',  ( -0.9730401042858022320, 0.2306359803922080343, 5.959266323858941219E-17 ) ) ;
#20573 = VERTEX_POINT ( 'NONE', #19415 ) ;
#20574 = CARTESIAN_POINT ( 'NONE',  ( -14.00000000000150102, -19.99999999944489915, -6.749999999996830091 ) ) ;
#20575 = CARTESIAN_POINT ( 'NONE',  ( 117.6809342291340101, -10.28413402209830174, -2.440468108021579940E-14 ) ) ;
#20576 = SHAPE_DEFINITION_REPRESENTATION ( #1493, #8415 ) ;
#20577 = ORIENTED_EDGE ( 'NONE', *, *, #8079, .T. ) ;
#20578 = VERTEX_POINT ( 'NONE', #15612 ) ;
#20579 = CARTESIAN_POINT ( 'NONE',  ( -26.99999999999959854, -31.09999999999999787, -22.00000000000000000 ) ) ;
#20580 = CARTESIAN_POINT ( 'NONE',  ( -59.87132660632070014, -21.81388311970430038, -5.000000000000000000 ) ) ;
#20581 = VECTOR ( 'NONE', #9365, 1000.000000000000000 ) ;
#20582 = ORIENTED_EDGE ( 'NONE', *, *, #19720, .F. ) ;
#20583 = APPROVAL_DATE_TIME ( #617, #20093 ) ;
#20584 = CARTESIAN_POINT ( 'NONE',  ( -14.98746859792150055, 26.70208920133150343, -7.999999999996709299 ) ) ;
#20585 = EDGE_CURVE ( 'NONE', #2245, #5079, #8855, .T. ) ;
#20586 = LOCAL_TIME ( 14, 11, 27.00000000000000000, #22535 ) ;
#20587 = FACE_OUTER_BOUND ( 'NONE', #3958, .T. ) ;
#20588 = CONTEXT_DEPENDENT_SHAPE_REPRESENTATION ( #1559, #2680 ) ;
#20589 = CIRCLE ( 'NONE', #18725, 2.499999999999999112 ) ;
#20590 = DIRECTION ( 'NONE',  ( 0.2306359803922076457, 0.9730401042858025651, 0.000000000000000000 ) ) ;
#20591 = AXIS2_PLACEMENT_3D ( 'NONE', #10792, #7552, #2195 ) ;
#20592 = EDGE_CURVE ( 'NONE', #14649, #13995, #16788, .T. ) ;
#20593 = AXIS2_PLACEMENT_3D ( 'NONE', #4221, #11496, #22507 ) ;
#20594 = CARTESIAN_POINT ( 'NONE',  ( 52.45828777336790694, 19.13776831658130106, 13.00000000000000000 ) ) ;
#20595 = ADVANCED_FACE ( 'NONE', ( #21186 ), #10291, .F. ) ;
#20596 = FACE_OUTER_BOUND ( 'NONE', #9066, .T. ) ;
#20597 = APPLICATION_PROTOCOL_DEFINITION ( 'international standard', 'config_control_design', 1994, #21555 ) ;
#20598 = EDGE_CURVE ( 'NONE', #23191, #7012, #23192, .T. ) ;
#20599 = LINE ( 'NONE', #22357, #13811 ) ;
#20600 = AXIS2_PLACEMENT_3D ( 'NONE', #8385, #17762, #6617 ) ;
#20601 = DIRECTION ( 'NONE',  ( -6.281952996264309889E-17, -4.969341027148640384E-15, -1.000000000000000000 ) ) ;
#20602 = AXIS2_PLACEMENT_3D ( 'NONE', #11410, #22539, #20527 ) ;
#20603 = DIRECTION ( 'NONE',  ( 0.000000000000000000, 0.000000000000000000, 1.000000000000000000 ) ) ;
#20604 = APPROVAL_PERSON_ORGANIZATION ( #22857, #23283, #13845 ) ;
#20605 = DIRECTION ( 'NONE',  ( 0.2306359803922030383, 0.9730401042858035643, -1.407521210652539229E-17 ) ) ;
#20606 = FACE_OUTER_BOUND ( 'NONE', #7592, .T. ) ;
#20607 = AXIS2_PLACEMENT_3D ( 'NONE', #696, #7960, #6176 ) ;
#20608 = DIRECTION ( 'NONE',  ( -2.056924381537025249E-14, 6.140746379865968924E-31, -1.000000000000000000 ) ) ;
#20609 = AXIS2_PLACEMENT_3D ( 'NONE', #17402, #21303, #22721 ) ;
#20610 = VERTEX_POINT ( 'NONE', #7075 ) ;
#20611 = AXIS2_PLACEMENT_3D ( 'NONE', #2173, #14762, #18346 ) ;
#20612 = VERTEX_POINT ( 'NONE', #21529 ) ;
#20613 = FACE_OUTER_BOUND ( 'NONE', #10629, .T. ) ;
#20614 = LINE ( 'NONE', #13367, #4138 ) ;
#20615 = ORIENTED_EDGE ( 'NONE', *, *, #17100, .F. ) ;
#20616 = DIRECTION ( 'NONE',  ( -0.2306359803922033991, -0.9730401042858034533, 0.000000000000000000 ) ) ;
#20617 = ORIENTED_EDGE ( 'NONE', *, *, #1217, .T. ) ;
#20618 = LINE ( 'NONE', #539, #16663 ) ;
#20619 = AXIS2_PLACEMENT_3D ( 'NONE', #20205, #21850, #3933 ) ;
#20620 = APPROVAL_DATE_TIME ( #7673, #12579 ) ;
#20621 = DIRECTION ( 'NONE',  ( -0.7071067811865475727, 0.000000000000000000, -0.7071067811865475727 ) ) ;
#20622 = CC_DESIGN_SECURITY_CLASSIFICATION ( #5445, ( #23474 ) ) ;
#20623 = VECTOR ( 'NONE', #15037, 1000.000000000000227 ) ;
#20624 = DATE_TIME_ROLE ( 'classification_date' ) ;
#20625 = AXIS2_PLACEMENT_3D ( 'NONE', #21548, #5284, #3387 ) ;
#20626 = CARTESIAN_POINT ( 'NONE',  ( 117.1011158151309957, -12.73035498497280038, -19.59999999999999787 ) ) ;
#20627 = ORIENTED_EDGE ( 'NONE', *, *, #6612, .T. ) ;
#20628 = VECTOR ( 'NONE', #17424, 1000.000000000000000 ) ;
#20629 = CARTESIAN_POINT ( 'NONE',  ( 39.74442752440959481, 5.605205456207779768, -20.00000000000000000 ) ) ;
#20630 = ORIENTED_EDGE ( 'NONE', *, *, #22705, .F. ) ;
#20631 = CARTESIAN_POINT ( 'NONE',  ( 26.57755037370658613, -6.586732293729981258, 13.00000000000000000 ) ) ;
#20632 = DIRECTION ( 'NONE',  ( 1.000000000000000000, -2.270069654138870255E-15, 3.099353312215988811E-62 ) ) ;
#20633 = ORIENTED_EDGE ( 'NONE', *, *, #22410, .T. ) ;
#20634 = CARTESIAN_POINT ( 'NONE',  ( 5.000000000000000000, -31.09999999999999787, 2.500000000000000000 ) ) ;
#20635 = CARTESIAN_POINT ( 'NONE',  ( 33.91471097434123294, 19.16532731944443313, -13.00000000000049916 ) ) ;
#20636 = VERTEX_POINT ( 'NONE', #17756 ) ;
#20637 = EDGE_CURVE ( 'NONE', #12862, #11256, #3148, .T. ) ;
#20638 = AXIS2_PLACEMENT_3D ( 'NONE', #16793, #520, #7775 ) ;
#20639 = APPROVAL_ROLE ( '' ) ;
#20640 = CONICAL_SURFACE ( 'NONE', #10425, 1.033499999999999863, 1.029744258676650093 ) ;
#20641 = ORIENTED_EDGE ( 'NONE', *, *, #15033, .T. ) ;
#20642 = COORDINATED_UNIVERSAL_TIME_OFFSET ( 0, 0, .AHEAD. ) ;
#20643 = DIRECTION ( 'NONE',  ( -6.662111338785949120E-09, 1.000000000000000000, -1.982541115402066096E-15 ) ) ;
#20644 = VERTEX_POINT ( 'NONE', #15961 ) ;
#20645 = EDGE_LOOP ( 'NONE', ( #4284, #13676, #7679, #6824 ) ) ;
#20646 = DATE_AND_TIME ( #9847, #20586 ) ;
#20647 = DATE_AND_TIME ( #681, #5367 ) ;
#20648 = DIRECTION ( 'NONE',  ( -0.2306359803922076457, -0.9730401042858024541, 1.412237191019896446E-17 ) ) ;
#20649 = CYLINDRICAL_SURFACE ( 'NONE', #14532, 5.000000000000000888 ) ;
#20650 = ORIENTED_EDGE ( 'NONE', *, *, #7973, .F. ) ;
#20651 = DATE_AND_TIME ( #4734, #371 ) ;
#20652 = EDGE_LOOP ( 'NONE', ( #14845, #14329, #13777, #8613 ) ) ;
#20653 = FACE_OUTER_BOUND ( 'NONE', #20043, .T. ) ;
#20654 = CARTESIAN_POINT ( 'NONE',  ( 114.2412296582674429, -24.79605227811687485, -13.00000000000000000 ) ) ;
#20655 = ORIENTED_EDGE ( 'NONE', *, *, #23468, .T. ) ;
#20656 = ADVANCED_FACE ( 'NONE', ( #6963 ), #21428, .T. ) ;
#20657 = CARTESIAN_POINT ( 'NONE',  ( -27.00000000000000000, -29.85000000000000142, 12.00000000000000000 ) ) ;
#20658 = DIRECTION ( 'NONE',  ( -0.9730401042858024541, 0.2306359803922080898, 5.959266323858942451E-17 ) ) ;
#20659 = DIRECTION ( 'NONE',  ( -0.04564792618500997101, -0.9989575901083128651, 2.775557561562890562E-15 ) ) ;
#20660 = ORIENTED_EDGE ( 'NONE', *, *, #9286, .F. ) ;
#20661 = VERTEX_POINT ( 'NONE', #2909 ) ;
#20662 = CARTESIAN_POINT ( 'NONE',  ( -68.53146193154570653, -21.85922789657999843, -2.680796741387739937E-15 ) ) ;
#20663 = ORIENTED_EDGE ( 'NONE', *, *, #8474, .T. ) ;
#20664 = CALENDAR_DATE ( 2026, 31, 10 ) ;
#20665 = EDGE_LOOP ( 'NONE', ( #8910, #14724, #3486, #8784 ) ) ;
#20666 = ORIENTED_EDGE ( 'NONE', *, *, #18867, .F. ) ;
#20667 = DIRECTION ( 'NONE',  ( 0.9999862922474493931, 0.005235963827108502076, 0.000000000000000000 ) ) ;
#20668 = PERSON_AND_ORGANIZATION ( #11966, #8758 ) ;
#20669 = EDGE_CURVE ( 'NONE', #14097, #10685, #11757, .T. ) ;
#20670 = LINE ( 'NONE', #2257, #5549 ) ;
#20671 = ADVANCED_FACE ( 'NONE', ( #19187, #13842 ), #12989, .T. ) ;
#20672 = DIRECTION ( 'NONE',  ( -0.9730401042858035643, 0.2306359803922028717, 5.432877459303547053E-17 ) ) ;
#20673 = DIRECTION ( 'NONE',  ( 0.000000000000000000, 0.000000000000000000, 1.000000000000000000 ) ) ;
#20674 = PERSON ( 'NAUO-PER20', 'UNSPECIFIED', 'UNSPECIFIED', ('UNSPECIFIED'), ('UNSPECIFIED'), ('UNSPECIFIED') ) ;
#20675 = CARTESIAN_POINT ( 'NONE',  ( -30.79248430819439974, 6.338858557519089665, -2.999000000000079602 ) ) ;
#20676 = PERSON_AND_ORGANIZATION_ROLE ( 'creator' ) ;
#20677 = CIRCLE ( 'NONE', #5511, 8.250000000000001776 ) ;
#20678 =( BOUNDED_CURVE ( )  B_SPLINE_CURVE ( 2, ( #17037, #13600, #6468 ),
 .UNSPECIFIED., .F., .F. ) 
 B_SPLINE_CURVE_WITH_KNOTS ( ( 3, 3 ),
 ( 0.000000000000000000, 0.2336872276155859962 ),
 .UNSPECIFIED. ) 
 CURVE ( )  GEOMETRIC_REPRESENTATION_ITEM ( )  RATIONAL_B_SPLINE_CURVE ( ( 1.000000000000000000, 1.154700538379259900, 1.000000000000000000 ) ) 
 REPRESENTATION_ITEM ( '' )  );
#20679 = VERTEX_POINT ( 'NONE', #5267 ) ;
#20680 = CARTESIAN_POINT ( 'NONE',  ( 35.63933253682661473, 8.222551437987098311, -27.55602540378493970 ) ) ;
#20681 = DIRECTION ( 'NONE',  ( 0.2306359803922085339, 0.9730401042858022320, 0.000000000000000000 ) ) ;
#20682 = VERTEX_POINT ( 'NONE', #16426 ) ;
#20683 = EDGE_CURVE ( 'NONE', #14652, #6743, #16304, .T. ) ;
#20684 = DIRECTION ( 'NONE',  ( -0.9999862922474493931, -0.005235963827108232327, 7.691850745534263154E-16 ) ) ;
#20685 = CARTESIAN_POINT ( 'NONE',  ( 120.8697533057606961, 5.046729969097242474, 13.00000000000000000 ) ) ;
#20686 = VERTEX_POINT ( 'NONE', #5386 ) ;
#20687 = FACE_OUTER_BOUND ( 'NONE', #11016, .T. ) ;
#20688 = PRODUCT_RELATED_PRODUCT_CATEGORY ( 'detail', '', ( #13292 ) ) ;
#20689 = PERSON_AND_ORGANIZATION ( #11966, #8758 ) ;
#20690 = PRODUCT_DEFINITION_SHAPE ( 'NONE', 'NONE',  #18095 ) ;
#20691 = ORIENTED_EDGE ( 'NONE', *, *, #3745, .T. ) ;
#20692 = CC_DESIGN_DATE_AND_TIME_ASSIGNMENT ( #20863, #10084, ( #18531 ) ) ;
#20693 = EDGE_LOOP ( 'NONE', ( #10359, #377 ) ) ;
#20694 = LINE ( 'NONE', #22579, #13018 ) ;
#20695 = CARTESIAN_POINT ( 'NONE',  ( 43.98050001724070057, -5.573152644851429471, -10.50000000000039968 ) ) ;
#20696 = ORIENTED_EDGE ( 'NONE', *, *, #15419, .T. ) ;
#20697 = CALENDAR_DATE ( 2026, 31, 10 ) ;
#20698 = ADVANCED_FACE ( 'NONE', ( #27, #12655 ), #151, .T. ) ;
#20699 = CARTESIAN_POINT ( 'NONE',  ( 118.6002496876800052, -6.405594307115129560, 18.89999999999999858 ) ) ;
#20700 = ADVANCED_FACE ( 'NONE', ( #19889 ), #1817, .T. ) ;
#20701 = CIRCLE ( 'NONE', #581, 2.500000000000001332 ) ;
#20702 = ADVANCED_FACE ( 'NONE', ( #11108 ), #16806, .T. ) ;
#20703 = PLANE ( 'NONE',  #386 ) ;
#20704 = CALENDAR_DATE ( 2026, 31, 10 ) ;
#20705 = DIRECTION ( 'NONE',  ( -9.594916218540590128E-33, 2.583840697242805182E-16, -1.000000000000000000 ) ) ;
#20706 = AXIS2_PLACEMENT_3D ( 'NONE', #20050, #14706, #12595 ) ;
#20707 = DIRECTION ( 'NONE',  ( -3.099353312215989243E-62, -9.818186930595456717E-93, 1.000000000000000000 ) ) ;
#20708 = SHAPE_DEFINITION_REPRESENTATION ( #22924, #1735 ) ;
#20709 = CARTESIAN_POINT ( 'NONE',  ( 113.4570673249340018, -28.10438863268850085, -3.399999999999949729 ) ) ;
#20710 = CARTESIAN_POINT ( 'NONE',  ( 33.37436288052550282, -3.059220458576419777, -13.00000000000039968 ) ) ;
#20711 = FACE_OUTER_BOUND ( 'NONE', #19855, .T. ) ;
#20712 = EDGE_CURVE ( 'NONE', #21153, #2245, #9431, .T. ) ;
#20713 =( GEOMETRIC_REPRESENTATION_CONTEXT ( 3 ) GLOBAL_UNCERTAINTY_ASSIGNED_CONTEXT ( ( #15843 ) ) GLOBAL_UNIT_ASSIGNED_CONTEXT ( ( #14771, #16653, #4788 ) ) REPRESENTATION_CONTEXT ( 'NONE', 'WORKASPACE' ) );
#20714 = DIRECTION ( 'NONE',  ( -0.2306359803922033991, -0.9730401042858034533, 0.000000000000000000 ) ) ;
#20715 = CARTESIAN_POINT ( 'NONE',  ( -20.00000000000000000, -20.00000000000000000, -2.500000000000000000 ) ) ;
#20716 = ORIENTED_EDGE ( 'NONE', *, *, #7929, .F. ) ;
#20717 = EDGE_LOOP ( 'NONE', ( #21022, #1628 ) ) ;
#20718 = DIRECTION ( 'NONE',  ( -0.2306359803922081175, -0.9730401042858022320, 1.412237191019896138E-17 ) ) ;
#20719 = CARTESIAN_POINT ( 'NONE',  ( 35.59419854219520118, 9.774809681453278998, -26.30000000000050164 ) ) ;
#20720 = VERTEX_POINT ( 'NONE', #379 ) ;
#20721 = EDGE_CURVE ( 'NONE', #184, #3145, #22502, .T. ) ;
#20722 = CARTESIAN_POINT ( 'NONE',  ( 11.50000000000000000, -23.36217782649120167, 5.000000000000000000 ) ) ;
#20723 = EDGE_CURVE ( 'NONE', #10381, #18788, #3536, .T. ) ;
#20724 = ORIENTED_EDGE ( 'NONE', *, *, #6654, .F. ) ;
#20725 = DIRECTION ( 'NONE',  ( 4.028143194477080210E-16, 2.054129435991050111E-15, 1.000000000000000000 ) ) ;
#20726 = PERSON_AND_ORGANIZATION ( #11966, #8758 ) ;
#20727 = DIRECTION ( 'NONE',  ( 0.8660135325225010172, 0.004534477687579660174, 0.5000000000000000000 ) ) ;
#20728 = CIRCLE ( 'NONE', #3288, 2.499999999999998668 ) ;
#20729 = COORDINATED_UNIVERSAL_TIME_OFFSET ( 0, 0, .AHEAD. ) ;
#20730 = AXIS2_PLACEMENT_3D ( 'NONE', #1334, #10405, #17632 ) ;
#20731 = LINE ( 'NONE', #543, #1044 ) ;
#20732 = CARTESIAN_POINT ( 'NONE',  ( -20.00000000397270128, 22.95208919257159863, 5.500000000004459544 ) ) ;
#20733 = ORIENTED_EDGE ( 'NONE', *, *, #20747, .T. ) ;
#20734 = LINE ( 'NONE', #18619, #4113 ) ;
#20735 = EDGE_CURVE ( 'NONE', #5237, #4833, #4307, .T. ) ;
#20736 = DIRECTION ( 'NONE',  ( 0.000000000000000000, 0.000000000000000000, -1.000000000000000000 ) ) ;
#20737 = VERTEX_POINT ( 'NONE', #9191 ) ;
#20738 = CIRCLE ( 'NONE', #2154, 2.500000000000000888 ) ;
#20739 = DIRECTION ( 'NONE',  ( 0.8846153846153640421, -0.4663213712685829182, 0.000000000000000000 ) ) ;
#20740 = CARTESIAN_POINT ( 'NONE',  ( -19.49999999982360066, -0.1021026942259609938, 3.750000000000000000 ) ) ;
#20741 = UNCERTAINTY_MEASURE_WITH_UNIT (LENGTH_MEASURE( 1.000000000000000082E-05 ), #1653, 'distance_accuracy_value', 'NONE');
#20742 = ADVANCED_FACE ( 'NONE', ( #9070 ), #12758, .F. ) ;
#20743 = AXIS2_PLACEMENT_3D ( 'NONE', #15513, #13972, #19433 ) ;
#20744 = COORDINATED_UNIVERSAL_TIME_OFFSET ( 0, 0, .AHEAD. ) ;
#20745 = DIRECTION ( 'NONE',  ( -0.9730401042858020100, 0.2306359803922089780, -1.063156381331940130E-15 ) ) ;
#20746 = AXIS2_PLACEMENT_3D ( 'NONE', #16179, #20089, #14525 ) ;
#20747 = EDGE_CURVE ( 'NONE', #8958, #10146, #23090, .T. ) ;
#20748 = ORIENTED_EDGE ( 'NONE', *, *, #19611, .F. ) ;
#20749 = ADVANCED_FACE ( 'NONE', ( #12867 ), #20109, .F. ) ;
#20750 = DATE_AND_TIME ( #15764, #17523 ) ;
#20751 = DIRECTION ( 'NONE',  ( 0.9730401042858036753, -0.2306359803922031493, 2.804983810440361760E-16 ) ) ;
#20752 = EDGE_LOOP ( 'NONE', ( #7039, #7727, #6602, #17088 ) ) ;
#20753 = ORIENTED_EDGE ( 'NONE', *, *, #6267, .T. ) ;
#20754 = VECTOR ( 'NONE', #3493, 999.9999999999998863 ) ;
#20755 = APPROVAL_STATUS ( 'not_yet_approved' ) ;
#20756 = DATE_AND_TIME ( #15406, #16360 ) ;
#20757 = CIRCLE ( 'NONE', #10542, 4.250000000000000000 ) ;
#20758 = DIRECTION ( 'NONE',  ( 0.1153179901961009640, 0.4865200521429018377, -0.8660254037844385966 ) ) ;
#20759 = AXIS2_PLACEMENT_3D ( 'NONE', #18117, #3848, #19661 ) ;
#20760 = AXIS2_PLACEMENT_3D ( 'NONE', #7423, #21886, #4081 ) ;
#20761 = AXIS2_PLACEMENT_3D ( 'NONE', #1186, #14024, #1309 ) ;
#20762 = PLANE ( 'NONE',  #21722 ) ;
#20763 = ORIENTED_EDGE ( 'NONE', *, *, #11595, .T. ) ;
#20764 = APPLICATION_PROTOCOL_DEFINITION ( 'international standard', 'config_control_design', 1994, #17171 ) ;
#20765 = ORIENTED_EDGE ( 'NONE', *, *, #21632, .T. ) ;
#20766 = CIRCLE ( 'NONE', #8272, 5.000000000000002665 ) ;
#20767 = CARTESIAN_POINT ( 'NONE',  ( 33.37436288052550282, -3.059220458576299873, 13.00000000000019895 ) ) ;
#20768 = DIRECTION ( 'NONE',  ( 2.982858504489139758E-17, -2.441916418604790135E-15, -1.000000000000000000 ) ) ;
#20769 = EDGE_LOOP ( 'NONE', ( #17250, #844 ) ) ;
#20770 = PRODUCT_DEFINITION ( 'UNKNOWN', '', #14461, #368 ) ;
#20771 = FACE_OUTER_BOUND ( 'NONE', #13395, .T. ) ;
#20772 = DIRECTION ( 'NONE',  ( -2.269747459788994803E-13, -2.220446049250605354E-15, -1.000000000000000000 ) ) ;
#20773 = DIRECTION ( 'NONE',  ( 0.9730401042858035643, -0.2306359803922028717, -5.958148513035547083E-17 ) ) ;
#20774 = AXIS2_PLACEMENT_3D ( 'NONE', #13529, #6655, #3073 ) ;
#20775 = EDGE_LOOP ( 'NONE', ( #17644, #2130, #10258, #19291 ) ) ;
#20776 = VERTEX_POINT ( 'NONE', #16535 ) ;
#20777 = DIRECTION ( 'NONE',  ( -1.164423685541379998E-14, -4.938475812832819565E-14, 1.000000000000000000 ) ) ;
#20778 = ORIENTED_EDGE ( 'NONE', *, *, #16374, .T. ) ;
#20779 = COORDINATED_UNIVERSAL_TIME_OFFSET ( 0, 0, .AHEAD. ) ;
#20780 = CIRCLE ( 'NONE', #281, 2.500000000028980374 ) ;
#20781 = ORIENTED_EDGE ( 'NONE', *, *, #13415, .F. ) ;
#20782 = VERTEX_POINT ( 'NONE', #7181 ) ;
#20783 = CARTESIAN_POINT ( 'NONE',  ( -65.63554743930404811, 13.34974264280344514, -5.515482965309170069E-15 ) ) ;
#20784 = AXIS2_PLACEMENT_3D ( 'NONE', #18005, #21654, #16316 ) ;
#20785 = DATE_AND_TIME ( #13439, #17904 ) ;
#20786 = DIRECTION ( 'NONE',  ( 0.000000000000000000, 1.668003342285391304E-16, 1.000000000000000000 ) ) ;
#20787 = EDGE_CURVE ( 'NONE', #12644, #10034, #17590, .T. ) ;
#20788 =( NAMED_UNIT ( * ) SI_UNIT ( $, .STERADIAN. ) SOLID_ANGLE_UNIT ( ) );
#20789 = VECTOR ( 'NONE', #22267, 1000.000000000000000 ) ;
#20790 = CARTESIAN_POINT ( 'NONE',  ( -65.80336369117380002, 8.448563927732790191, 5.000000000000000000 ) ) ;
#20791 = SHAPE_DEFINITION_REPRESENTATION ( #14404, #10862 ) ;
#20792 = CIRCLE ( 'NONE', #6392, 5.000000000000004441 ) ;
#20793 = ORIENTED_EDGE ( 'NONE', *, *, #10155, .F. ) ;
#20794 = CARTESIAN_POINT ( 'NONE',  ( 118.4388045014059969, -7.086722380115130449, 19.59999999999999787 ) ) ;
#20795 = DIRECTION ( 'NONE',  ( 0.000000000000000000, 0.000000000000000000, 1.000000000000000000 ) ) ;
#20796 = VERTEX_POINT ( 'NONE', #260 ) ;
#20797 = ADVANCED_FACE ( 'NONE', ( #10768 ), #8963, .T. ) ;
#20798 = EDGE_CURVE ( 'NONE', #13304, #2609, #9791, .T. ) ;
#20799 = CARTESIAN_POINT ( 'NONE',  ( 39.27359436029429673, 22.26288585089420025, -13.00000000000049916 ) ) ;
#20800 = CARTESIAN_POINT ( 'NONE',  ( 0.9301579624205805752, 15.86682475602536257, -7.031157038775623375E-15 ) ) ;
#20801 = VERTEX_POINT ( 'NONE', #18579 ) ;
#20802 = CARTESIAN_POINT ( 'NONE',  ( 43.45766680872420551, 21.27115113520920175, -13.00000000000000000 ) ) ;
#20803 = APPLICATION_CONTEXT ( 'configuration controlled 3d designs of mechanical parts and assemblies' ) ;
#20804 = DATE_TIME_ROLE ( 'classification_date' ) ;
#20805 = VERTEX_POINT ( 'NONE', #728 ) ;
#20806 = ORIENTED_EDGE ( 'NONE', *, *, #11257, .F. ) ;
#20807 = CARTESIAN_POINT ( 'NONE',  ( 34.54155158422950223, 23.97785071899690124, -15.00000000000049916 ) ) ;
#20808 = CARTESIAN_POINT ( 'NONE',  ( -4.514225866272970400, 4.676725866273559795, -5.000000000000000000 ) ) ;
#20809 = ORIENTED_EDGE ( 'NONE', *, *, #400, .T. ) ;
#20810 = PERSON_AND_ORGANIZATION ( #11966, #8758 ) ;
#20811 = DIRECTION ( 'NONE',  ( 0.2306359803922080620, 0.9730401042858023430, -2.572202231434326974E-16 ) ) ;
#20812 = CLOSED_SHELL ( 'NONE', ( #8101, #9456, #9968, #18002, #8941, #20026 ) ) ;
#20813 = CARTESIAN_POINT ( 'NONE',  ( 34.03302451342609913, 9.759458723927547652, 29.25000000000000000 ) ) ;
#20814 = AXIS2_PLACEMENT_3D ( 'NONE', #20675, #17463, #951 ) ;
#20815 = DIRECTION ( 'NONE',  ( 0.000000000000000000, 0.5102823824563427202, -0.8600069128528436968 ) ) ;
#20816 = EDGE_CURVE ( 'NONE', #11662, #12727, #7343, .T. ) ;
#20817 = SHAPE_REPRESENTATION ( '1602p_c_08', ( #12739 ), #23107 ) ;
#20818 = CIRCLE ( 'NONE', #21623, 7.000000000000000888 ) ;
#20819 = PRODUCT_DEFINITION ( 'UNKNOWN', '', #6956, #13968 ) ;
#20820 = FACE_OUTER_BOUND ( 'NONE', #17133, .T. ) ;
#20821 = COORDINATED_UNIVERSAL_TIME_OFFSET ( 0, 0, .AHEAD. ) ;
#20822 = PRODUCT_RELATED_PRODUCT_CATEGORY ( 'detail', '', ( #3402 ) ) ;
#20823 = CARTESIAN_POINT ( 'NONE',  ( 36.44273712271338894, 7.885218776542735952, 8.849098278953681174 ) ) ;
#20824 = DIRECTION ( 'NONE',  ( 6.123230199561429643E-17, 4.868008300101910084E-15, 1.000000000000000000 ) ) ;
#20825 = EDGE_CURVE ( 'NONE', #18569, #16977, #4540, .T. ) ;
#20826 = ADVANCED_FACE ( 'NONE', ( #15353 ), #22103, .T. ) ;
#20827 = FACE_OUTER_BOUND ( 'NONE', #11744, .T. ) ;
#20828 = CARTESIAN_POINT ( 'NONE',  ( -5.657453702850906652, 21.67680139518235549, -1.552841462206820572E-15 ) ) ;
#20829 = CARTESIAN_POINT ( 'NONE',  ( -55.82882037092589655, -8.292431354569981039, 7.200000000000000178 ) ) ;
#20830 = CARTESIAN_POINT ( 'NONE',  ( -25.64161990512560152, 6.365892616704879714, 5.000000000000000000 ) ) ;
#20831 = ORIENTED_EDGE ( 'NONE', *, *, #21029, .F. ) ;
#20832 = ORIENTED_EDGE ( 'NONE', *, *, #6330, .T. ) ;
#20833 = DIRECTION ( 'NONE',  ( 0.9949874374308176339, 0.09999999677427344469, -2.262079412673755946E-13 ) ) ;
#20834 = CYLINDRICAL_SURFACE ( 'NONE', #15514, 2.500000000000001776 ) ;
#20835 = CARTESIAN_POINT ( 'NONE',  ( 33.37436288052550282, -3.059220458576419777, -13.00000000000039968 ) ) ;
#20836 = EDGE_LOOP ( 'NONE', ( #22931, #15129, #23089, #15166, #12498 ) ) ;
#20837 = VECTOR ( 'NONE', #11811, 999.9999999999998863 ) ;
#20838 = CARTESIAN_POINT ( 'NONE',  ( 1.883607105361947864, 19.88937254714287661, -6.836209472240241912E-15 ) ) ;
#20839 = ORIENTED_EDGE ( 'NONE', *, *, #14908, .F. ) ;
#20840 = FACE_OUTER_BOUND ( 'NONE', #11026, .T. ) ;
#20841 = DATE_AND_TIME ( #8511, #14139 ) ;
#20842 = CARTESIAN_POINT ( 'NONE',  ( 117.0319250210129951, -13.02226701625859917, 18.89999999999999858 ) ) ;
#20843 = ADVANCED_FACE ( 'NONE', ( #2290 ), #22583, .F. ) ;
#20844 = DIRECTION ( 'NONE',  ( -0.1997366180463769070, -0.8426774492125652660, 0.5000000000000002220 ) ) ;
#20845 = CC_DESIGN_PERSON_AND_ORGANIZATION_ASSIGNMENT ( #7940, #18639, ( #1530 ) ) ;
#20846 = LINE ( 'NONE', #15504, #295 ) ;
#20847 = CC_DESIGN_PERSON_AND_ORGANIZATION_ASSIGNMENT ( #20432, #16980, ( #16700 ) ) ;
#20848 = AXIS2_PLACEMENT_3D ( 'NONE', #9225, #16455, #174 ) ;
#20849 = CARTESIAN_POINT ( 'NONE',  ( 32.77470933150577537, -5.589124729719389784, 13.00000000000019895 ) ) ;
#20850 = CIRCLE ( 'NONE', #10269, 7.999999999999997335 ) ;
#20851 = VERTEX_POINT ( 'NONE', #20584 ) ;
#20852 = CYLINDRICAL_SURFACE ( 'NONE', #6358, 2.066999999999998394 ) ;
#20853 = EDGE_CURVE ( 'NONE', #20315, #10599, #5975, .T. ) ;
#20854 = EDGE_CURVE ( 'NONE', #104, #3196, #8128, .T. ) ;
#20855 = DIRECTION ( 'NONE',  ( 0.9730401042858035643, -0.2306359803922028717, -5.959266323858677443E-17 ) ) ;
#20856 = ORIENTED_EDGE ( 'NONE', *, *, #9417, .F. ) ;
#20857 = DIRECTION ( 'NONE',  ( -0.9730401042858036753, 0.2306359803922028995, 5.958148513035547083E-17 ) ) ;
#20858 = DIRECTION ( 'NONE',  ( 0.9730401042858036753, -0.2306359803922031493, 2.804983810440361760E-16 ) ) ;
#20859 = APPROVAL_ROLE ( '' ) ;
#20860 = DIRECTION ( 'NONE',  ( -1.159535895544890222E-14, -2.167612681253619929E-15, -1.000000000000000000 ) ) ;
#20861 = EDGE_LOOP ( 'NONE', ( #5475, #3082 ) ) ;
#20862 = ORIENTED_EDGE ( 'NONE', *, *, #6017, .F. ) ;
#20863 = DATE_AND_TIME ( #22883, #1188 ) ;
#20864 = DIRECTION ( 'NONE',  ( 3.210834492194360164E-17, -2.441916418604790135E-15, -1.000000000000000000 ) ) ;
#20865 = ORIENTED_EDGE ( 'NONE', *, *, #11412, .T. ) ;
#20866 = PRODUCT_DEFINITION_FORMATION_WITH_SPECIFIED_SOURCE ( 'ANY', '', #15527, .NOT_KNOWN. ) ;
#20867 = CARTESIAN_POINT ( 'NONE',  ( 39.37089837072289811, 22.23982225285509884, 13.00000000000000000 ) ) ;
#20868 =( GEOMETRIC_REPRESENTATION_CONTEXT ( 3 ) GLOBAL_UNCERTAINTY_ASSIGNED_CONTEXT ( ( #12981 ) ) GLOBAL_UNIT_ASSIGNED_CONTEXT ( ( #2012, #1358, #21196 ) ) REPRESENTATION_CONTEXT ( 'NONE', 'WORKASPACE' ) );
#20869 = DATE_AND_TIME ( #918, #3141 ) ;
#20870 = VECTOR ( 'NONE', #21668, 1000.000000000000000 ) ;
#20871 = EDGE_CURVE ( 'NONE', #13431, #15347, #971, .T. ) ;
#20872 = CALENDAR_DATE ( 2026, 31, 10 ) ;
#20873 = CARTESIAN_POINT ( 'NONE',  ( -68.70795112897079093, 11.84741790582710053, 3.773156417642989929E-15 ) ) ;
#20874 = VECTOR ( 'NONE', #1308, 1000.000000000000227 ) ;
#20875 = CARTESIAN_POINT ( 'NONE',  ( 36.34169561367309598, 12.92845737834490016, 29.25000000000000000 ) ) ;
#20876 = ORIENTED_EDGE ( 'NONE', *, *, #7750, .T. ) ;
#20877 = EDGE_CURVE ( 'NONE', #4635, #16195, #12291, .T. ) ;
#20878 = PERSON_AND_ORGANIZATION ( #11966, #8758 ) ;
#20879 = PRODUCT_DEFINITION_SHAPE ( 'NONE', 'NONE',  #5893 ) ;
#20880 = APPROVAL_PERSON_ORGANIZATION ( #9043, #21563, #14261 ) ;
#20881 = EDGE_CURVE ( 'NONE', #2884, #15102, #11594, .T. ) ;
#20882 = VERTEX_POINT ( 'NONE', #18820 ) ;
#20883 = APPROVAL_PERSON_ORGANIZATION ( #18812, #21286, #8119 ) ;
#20884 = CARTESIAN_POINT ( 'NONE',  ( 4.267766952966340455, -31.10000000000000142, 20.76776695296636532 ) ) ;
#20885 = DIRECTION ( 'NONE',  ( 0.000000000000000000, 0.000000000000000000, -1.000000000000000000 ) ) ;
#20886 = ORIENTED_EDGE ( 'NONE', *, *, #9877, .F. ) ;
#20887 = CARTESIAN_POINT ( 'NONE',  ( 103.2898377416287303, 9.213630226843337212, 13.00000000000000000 ) ) ;
#20888 = DIRECTION ( 'NONE',  ( -0.8823529412199658806, 0.4705882352125641543, 1.991462550421374292E-13 ) ) ;
#20889 = DIRECTION ( 'NONE',  ( -0.9997648975362233292, -0.02168293463497999313, 0.000000000000000000 ) ) ;
#20890 = ORIENTED_EDGE ( 'NONE', *, *, #18810, .T. ) ;
#20891 = VERTEX_POINT ( 'NONE', #22346 ) ;
#20892 = DIRECTION ( 'NONE',  ( -0.9730401042858024541, 0.2306359803922080898, 5.959266323858942451E-17 ) ) ;
#20893 = ORIENTED_EDGE ( 'NONE', *, *, #5454, .T. ) ;
#20894 = AXIS2_PLACEMENT_3D ( 'NONE', #20390, #6908, #10482 ) ;
#20895 = PERSON_AND_ORGANIZATION ( #11966, #8758 ) ;
#20896 = ORIENTED_EDGE ( 'NONE', *, *, #8939, .T. ) ;
#20897 = ORIENTED_EDGE ( 'NONE', *, *, #11986, .F. ) ;
#20898 = DIRECTION ( 'NONE',  ( 0.000000000000000000, 0.000000000000000000, -1.000000000000000000 ) ) ;
#20899 = SHAPE_DEFINITION_REPRESENTATION ( #4386, #9451 ) ;
#20900 = LOCAL_TIME ( 14, 11, 27.00000000000000000, #6778 ) ;
#20901 = LINE ( 'NONE', #12134, #11647 ) ;
#20902 = APPROVAL_PERSON_ORGANIZATION ( #20443, #18154, #16630 ) ;
#20903 = APPROVAL ( #22677, 'UNSPECIFIED' ) ;
#20904 = ORGANIZATION ( 'NAUO-ORG40', 'UNSPECIFIED', 'UNSPECIFIED' ) ;
#20905 = ORGANIZATION ( 'NAUO-ORG15', 'UNSPECIFIED', 'UNSPECIFIED' ) ;
#20906 = FACE_OUTER_BOUND ( 'NONE', #5479, .T. ) ;
#20907 = DATE_AND_TIME ( #832, #17460 ) ;
#20908 = ORIENTED_EDGE ( 'NONE', *, *, #118, .T. ) ;
#20909 = CARTESIAN_POINT ( 'NONE',  ( -65.64475015647069256, -21.84411297095480009, -5.000000000000000000 ) ) ;
#20910 = DIRECTION ( 'NONE',  ( -0.2306359803922101437, -0.9730401042858017879, 4.316864774682981680E-15 ) ) ;
#20911 = ORIENTED_EDGE ( 'NONE', *, *, #15600, .F. ) ;
#20912 = LOCAL_TIME ( 14, 11, 27.00000000000000000, #6327 ) ;
#20913 = LINE ( 'NONE', #10486, #1421 ) ;
#20914 = CARTESIAN_POINT ( 'NONE',  ( -20.80722593534541076, 19.54644882756858948, 2.500000000000000000 ) ) ;
#20915 = ORIENTED_EDGE ( 'NONE', *, *, #19009, .T. ) ;
#20916 = DIRECTION ( 'NONE',  ( -9.594916218540590128E-33, 2.583840697242805182E-16, -1.000000000000000000 ) ) ;
#20917 = AXIS2_PLACEMENT_3D ( 'NONE', #19691, #23116, #5440 ) ;
#20918 = AXIS2_PLACEMENT_3D ( 'NONE', #9517, #9284, #16509 ) ;
#20919 = COORDINATED_UNIVERSAL_TIME_OFFSET ( 0, 0, .AHEAD. ) ;
#20920 = EDGE_CURVE ( 'NONE', #21997, #2666, #2647, .T. ) ;
#20921 = ORIENTED_EDGE ( 'NONE', *, *, #7613, .T. ) ;
#20922 = VERTEX_POINT ( 'NONE', #16896 ) ;
#20923 = FACE_OUTER_BOUND ( 'NONE', #3110, .T. ) ;
#20924 = DIRECTION ( 'NONE',  ( -0.9730401042858036753, 0.2306359803922023999, 0.000000000000000000 ) ) ;
#20925 = CC_DESIGN_SECURITY_CLASSIFICATION ( #1200, ( #23501 ) ) ;
#20926 = VERTEX_POINT ( 'NONE', #17014 ) ;
#20927 = APPROVAL_ROLE ( '' ) ;
#20928 = DIRECTION ( 'NONE',  ( -1.751019220569994795E-16, -2.300154215587015208E-15, -1.000000000000000000 ) ) ;
#20929 = CYLINDRICAL_SURFACE ( 'NONE', #21136, 2.500000000000000000 ) ;
#20930 = ITEM_DEFINED_TRANSFORMATION ( 'NONE', 'NONE', #6459,  #10651 ) ;
#20931 = DIRECTION ( 'NONE',  ( 0.9730401042858024541, -0.2306359803922080898, -5.959266323858942451E-17 ) ) ;
#20932 = APPROVAL_PERSON_ORGANIZATION ( #11079, #21859, #16510 ) ;
#20933 = AXIS2_PLACEMENT_3D ( 'NONE', #1453, #14056, #1336 ) ;
#20934 = LINE ( 'NONE', #15477, #13597 ) ;
#20935 = PERSON_AND_ORGANIZATION ( #11966, #8758 ) ;
#20936 = AXIS2_PLACEMENT_3D ( 'NONE', #1376, #3180, #8645 ) ;
#20937 = AXIS2_PLACEMENT_3D ( 'NONE', #4827, #23334, #15756 ) ;
#20938 = CC_DESIGN_APPROVAL ( #6897, ( #17915 ) ) ;
#20939 = CARTESIAN_POINT ( 'NONE',  ( -69.90454993788326021, 6.134066389438223688, -0.7502499999999080460 ) ) ;
#20940 = CARTESIAN_POINT ( 'NONE',  ( 113.2033677465029911, -29.17473274740290279, -3.099999999999920153 ) ) ;
#20941 = VECTOR ( 'NONE', #607, 1000.000000000000114 ) ;
#20942 = DIRECTION ( 'NONE',  ( 1.138590270679730064E-14, 2.220446049251240387E-15, 1.000000000000000000 ) ) ;
#20943 = DIRECTION ( 'NONE',  ( 0.000000000000000000, -3.099353312215988811E-62, 1.000000000000000000 ) ) ;
#20944 = VECTOR ( 'NONE', #17703, 999.9999999999998863 ) ;
#20945 = DIRECTION ( 'NONE',  ( 1.227507208848341976E-15, 4.920447605136010024E-15, 1.000000000000000000 ) ) ;
#20946 = DIRECTION ( 'NONE',  ( -1.248400535696349791E-16, 3.446306084657139973E-17, 1.000000000000000000 ) ) ;
#20947 = ORIENTED_EDGE ( 'NONE', *, *, #15091, .T. ) ;
#20948 = EDGE_CURVE ( 'NONE', #12703, #13133, #10395, .T. ) ;
#20949 = LOCAL_TIME ( 14, 11, 27.00000000000000000, #5810 ) ;
#20950 = ORIENTED_EDGE ( 'NONE', *, *, #4318, .F. ) ;
#20951 = CARTESIAN_POINT ( 'NONE',  ( 5.000000000000000000, -27.34999999999999787, 5.000000000000000000 ) ) ;
#20952 = LINE ( 'NONE', #640, #19317 ) ;
#20953 = ORIENTED_EDGE ( 'NONE', *, *, #1385, .T. ) ;
#20954 = CIRCLE ( 'NONE', #20199, 2.066999999999997950 ) ;
#20955 = VECTOR ( 'NONE', #52, 1000.000000000000114 ) ;
#20956 = CC_DESIGN_DATE_AND_TIME_ASSIGNMENT ( #15879, #23347, ( #12227 ) ) ;
#20957 = DIRECTION ( 'NONE',  ( -0.2306359803922029550, -0.9730401042858035643, 4.741332172907960602E-18 ) ) ;
#20958 = ORIENTED_EDGE ( 'NONE', *, *, #22462, .F. ) ;
#20959 = AXIS2_PLACEMENT_3D ( 'NONE', #11144, #172, #14672 ) ;
#20960 = PLANE ( 'NONE',  #354 ) ;
#20961 =( BOUNDED_CURVE ( )  B_SPLINE_CURVE ( 2, ( #4520, #15335, #12027 ),
 .UNSPECIFIED., .F., .F. ) 
 B_SPLINE_CURVE_WITH_KNOTS ( ( 3, 3 ),
 ( 0.000000000000000000, 0.5842180690389578990 ),
 .UNSPECIFIED. ) 
 CURVE ( )  GEOMETRIC_REPRESENTATION_ITEM ( )  RATIONAL_B_SPLINE_CURVE ( ( 1.000000000000000000, 1.154700538379249908, 1.000000000000000000 ) ) 
 REPRESENTATION_ITEM ( '' )  );
#20962 = PERSON_AND_ORGANIZATION_ROLE ( 'creator' ) ;
#20963 = DIRECTION ( 'NONE',  ( -2.982858504577319616E-17, 2.441916418604790135E-15, 1.000000000000000000 ) ) ;
#20964 = ADVANCED_FACE ( 'NONE', ( #15237 ), #6204, .F. ) ;
#20965 = ADVANCED_FACE ( 'NONE', ( #10042, #9553, #13466 ), #16779, .T. ) ;
#20966 = VECTOR ( 'NONE', #2551, 1000.000000000000000 ) ;
#20967 = COORDINATED_UNIVERSAL_TIME_OFFSET ( 0, 0, .AHEAD. ) ;
#20968 = DIRECTION ( 'NONE',  ( 0.000000000000000000, 0.000000000000000000, 1.000000000000000000 ) ) ;
#20969 = CIRCLE ( 'NONE', #16032, 0.2000000000000012046 ) ;
#20971 = DIRECTION ( 'NONE',  ( -1.000000000000000000, 0.000000000000000000, 0.000000000000000000 ) ) ;
#20970 = AXIS2_PLACEMENT_3D ( 'NONE', #23139, #14135, #21379 ) ;
#20972 = CARTESIAN_POINT ( 'NONE',  ( 118.6002496876800052, -6.405594307115070052, -15.90000000000000036 ) ) ;
#20973 = SHAPE_REPRESENTATION_RELATIONSHIP ( 'NONE' , 'NONE' ,  #1735, #19008 ) ;
#20974 = CC_DESIGN_APPROVAL ( #23283, ( #5063 ) ) ;
#20975 = CARTESIAN_POINT ( 'NONE',  ( 37.01481097301077483, 22.79827665208023646, -15.00000000000051159 ) ) ;
#20976 = ORIENTED_EDGE ( 'NONE', *, *, #8508, .T. ) ;
#20977 = CARTESIAN_POINT ( 'NONE',  ( 105.8171986446039909, -20.23006919877430221, 13.00000000000000000 ) ) ;
#20978 = CONICAL_SURFACE ( 'NONE', #8091, 2.254620000000000068, 0.7853981633974461696 ) ;
#20979 = AXIS2_PLACEMENT_3D ( 'NONE', #4432, #9682, #11352 ) ;
#20980 = DIRECTION ( 'NONE',  ( -0.2306359803922080620, -0.9730401042858023430, -2.367063548676051037E-14 ) ) ;
#20981 = ORIENTED_EDGE ( 'NONE', *, *, #11346, .T. ) ;
#20982 = DIRECTION ( 'NONE',  ( -2.982858504577314686E-17, 2.441916418604790135E-15, 1.000000000000000000 ) ) ;
#20983 = FACE_BOUND ( 'NONE', #17067, .T. ) ;
#20984 = ADVANCED_FACE ( 'NONE', ( #17267 ), #8233, .T. ) ;
#20985 = SECURITY_CLASSIFICATION_LEVEL ( 'unclassified' ) ;
#20986 = FACE_OUTER_BOUND ( 'NONE', #1166, .T. ) ;
#20987 = ORIENTED_EDGE ( 'NONE', *, *, #1650, .F. ) ;
#20988 = AXIS2_PLACEMENT_3D ( 'NONE', #20594, #16541, #9561 ) ;
#20989 = ORIENTED_EDGE ( 'NONE', *, *, #14434, .F. ) ;
#20991 = SECURITY_CLASSIFICATION_LEVEL ( 'unclassified' ) ;
#20990 = CC_DESIGN_DATE_AND_TIME_ASSIGNMENT ( #17322, #20999, ( #7318 ) ) ;
#20992 = LINE ( 'NONE', #4603, #21687 ) ;
#20993 = LOCAL_TIME ( 14, 11, 27.00000000000000000, #4080 ) ;
#20994 = VECTOR ( 'NONE', #11738, 1000.000000000000000 ) ;
#20995 = ORIENTED_EDGE ( 'NONE', *, *, #13206, .F. ) ;
#20996 = CC_DESIGN_DATE_AND_TIME_ASSIGNMENT ( #18278, #9254, ( #10683 ) ) ;
#20997 = PLANE ( 'NONE',  #556 ) ;
#20998 =( REPRESENTATION_RELATIONSHIP ('NONE','NONE', #19303, #1388 ) REPRESENTATION_RELATIONSHIP_WITH_TRANSFORMATION ( #9730 )SHAPE_REPRESENTATION_RELATIONSHIP( ) );
#20999 = DATE_TIME_ROLE ( 'classification_date' ) ;
#21000 = VECTOR ( 'NONE', #13241, 1000.000000000000000 ) ;
#21001 = EDGE_CURVE ( 'NONE', #13190, #18417, #510, .T. ) ;
#21002 = EDGE_CURVE ( 'NONE', #3201, #2347, #19849, .T. ) ;
#21003 = CIRCLE ( 'NONE', #17544, 3.499999999999999556 ) ;
#21004 = CC_DESIGN_PERSON_AND_ORGANIZATION_ASSIGNMENT ( #13564, #9543, ( #19329 ) ) ;
#21005 = CALENDAR_DATE ( 2026, 31, 10 ) ;
#21006 = CARTESIAN_POINT ( 'NONE',  ( 34.14207834813680620, 22.29249582057189727, 11.00000000000000000 ) ) ;
#21007 = DIRECTION ( 'NONE',  ( -2.269747459788990007E-13, -2.220446049250330436E-15, -1.000000000000000000 ) ) ;
#21008 = ORIENTED_EDGE ( 'NONE', *, *, #22323, .F. ) ;
#21009 = COORDINATED_UNIVERSAL_TIME_OFFSET ( 0, 0, .AHEAD. ) ;
#21010 = CIRCLE ( 'NONE', #22130, 2.066999999999997506 ) ;
#21011 = EDGE_LOOP ( 'NONE', ( #16921, #16013 ) ) ;
#21012 = AXIS2_PLACEMENT_3D ( 'NONE', #15316, #9998, #933 ) ;
#21013 = PLANE ( 'NONE',  #3289 ) ;
#21014 = ORIENTED_EDGE ( 'NONE', *, *, #310, .F. ) ;
#21015 = ADVANCED_FACE ( 'NONE', ( #21163 ), #6929, .T. ) ;
#21016 = CARTESIAN_POINT ( 'NONE',  ( -25.64168762722610140, 6.365828311191170208, -2.500000000000000000 ) ) ;
#21017 = CARTESIAN_POINT ( 'NONE',  ( 2.500000000000000000, -30.47499999999999787, -19.00000000000000000 ) ) ;
#21018 = DIRECTION ( 'NONE',  ( 0.000000000000000000, 1.000000000000000000, 0.000000000000000000 ) ) ;
#21019 = ORIENTED_EDGE ( 'NONE', *, *, #18742, .F. ) ;
#21020 = ORIENTED_EDGE ( 'NONE', *, *, #11631, .T. ) ;
#21021 = CARTESIAN_POINT ( 'NONE',  ( -20.00479999606049830, 1.846597379377929782, 5.500000000004510170 ) ) ;
#21022 = ORIENTED_EDGE ( 'NONE', *, *, #20099, .T. ) ;
#21023 = CALENDAR_DATE ( 2026, 31, 10 ) ;
#21024 = EDGE_LOOP ( 'NONE', ( #21209, #20102, #2703, #10380 ) ) ;
#21025 = ORIENTED_EDGE ( 'NONE', *, *, #17901, .F. ) ;
#21026 = FACE_OUTER_BOUND ( 'NONE', #17232, .T. ) ;
#21027 = DATE_TIME_ROLE ( 'classification_date' ) ;
#21028 = EDGE_CURVE ( 'NONE', #19462, #2884, #22942, .T. ) ;
#21029 = EDGE_CURVE ( 'NONE', #9398, #11214, #13786, .T. ) ;
#21030 = DIRECTION ( 'NONE',  ( -1.466984912809907930E-16, -2.805478249466195144E-20, -1.000000000000000000 ) ) ;
#21031 = CYLINDRICAL_SURFACE ( 'NONE', #7714, 2.750000000000000888 ) ;
#21032 = DIRECTION ( 'NONE',  ( 0.000000000000000000, 1.020425574104004122E-16, 1.000000000000000000 ) ) ;
#21033 = APPROVAL_DATE_TIME ( #20907, #14233 ) ;
#21034 = PRODUCT ( '1602p_c_22', '1602p_c_22', '', ( #22756 ) ) ;
#21035 = ORIENTED_EDGE ( 'NONE', *, *, #16961, .F. ) ;
#21036 = CARTESIAN_POINT ( 'NONE',  ( 5.000000000000000000, -27.34999999999999787, 6.250000000000000000 ) ) ;
#21037 = CARTESIAN_POINT ( 'NONE',  ( -2.500000000000000000, 0.000000000000000000, -5.000000000000000000 ) ) ;
#21038 = VERTEX_POINT ( 'NONE', #1203 ) ;
#21039 = DIRECTION ( 'NONE',  ( 0.000000000000000000, -2.098117411679737831E-16, -1.000000000000000000 ) ) ;
#21040 = FACE_OUTER_BOUND ( 'NONE', #2552, .T. ) ;
#21041 = CARTESIAN_POINT ( 'NONE',  ( 112.5523895830310011, 2.765522746992189251, -1.033499999999968111 ) ) ;
#21042 = ORIENTED_EDGE ( 'NONE', *, *, #12843, .T. ) ;
#21043 = LINE ( 'NONE', #19267, #17151 ) ;
#21044 = VECTOR ( 'NONE', #16279, 1000.000000000000000 ) ;
#21045 = CALENDAR_DATE ( 2026, 31, 10 ) ;
#21046 = VERTEX_POINT ( 'NONE', #4900 ) ;
#21047 = VERTEX_POINT ( 'NONE', #21404 ) ;
#21048 = DIRECTION ( 'NONE',  ( 0.000000000000000000, 0.000000000000000000, 1.000000000000000000 ) ) ;
#21049 = DIRECTION ( 'NONE',  ( 6.123230159571619958E-17, 0.000000000000000000, 1.000000000000000000 ) ) ;
#21050 = ADVANCED_FACE ( 'NONE', ( #5136 ), #3115, .T. ) ;
#21051 = DIRECTION ( 'NONE',  ( 1.000000000000000000, 0.000000000000000000, 0.000000000000000000 ) ) ;
#21052 = COORDINATED_UNIVERSAL_TIME_OFFSET ( 0, 0, .AHEAD. ) ;
#21053 = EDGE_CURVE ( 'NONE', #16463, #1745, #12657, .T. ) ;
#21054 = DIRECTION ( 'NONE',  ( -0.07397971354964476276, -0.9972597464969256142, 2.428612866367529538E-15 ) ) ;
#21055 = DIRECTION ( 'NONE',  ( 0.000000000000000000, 1.000000000000000000, 0.000000000000000000 ) ) ;
#21056 = DIRECTION ( 'NONE',  ( 0.2306359803922085339, 0.9730401042858022320, 0.000000000000000000 ) ) ;
#21057 = AXIS2_PLACEMENT_3D ( 'NONE', #15717, #14825, #9743 ) ;
#21058 = B_SPLINE_CURVE_WITH_KNOTS ( 'NONE', 3,
 ( #2466, #773, #13393, #8044, #8283, #17665, #3277, #8397, #17421, #10198, #21091, #6626, #22980, #3169, #19316, #4945, #3041, #1259, #15755, #6987, #1130, #1479, #8744, #15636, #13739, #22876, #15980, #10312, #17309, #12213 ),
 .UNSPECIFIED., .F., .F.,
 ( 4, 2, 2, 2, 2, 2, 2, 2, 2, 2, 2, 2, 2, 2, 4 ),
 ( 0.006516123109207627717, 0.006923489735540700948, 0.007330856361873773312, 0.007738222988206846543, 0.008145589614539918907, 0.008960322867206065370, 0.009367689493539138601, 0.009775056119872211832, 0.01018242274620528506, 0.01058978937253835656, 0.01140452262520452037, 0.01181188925153760054, 0.01221925587787068071, 0.01262662250420376261, 0.01303398913053684278 ),
 .UNSPECIFIED. ) ;
#21059 = DIRECTION ( 'NONE',  ( -0.9730401042858035643, 0.2306359803922028717, 5.958148513035547083E-17 ) ) ;
#21060 = CALENDAR_DATE ( 2026, 31, 10 ) ;
#21061 = DIRECTION ( 'NONE',  ( 0.000000000000000000, 1.000000000000000000, 0.000000000000000000 ) ) ;
#21062 = FACE_OUTER_BOUND ( 'NONE', #9869, .T. ) ;
#21063 = CARTESIAN_POINT ( 'NONE',  ( -20.36989857172092044, 17.96579046008427127, -5.499999999995548450 ) ) ;
#21064 = CARTESIAN_POINT ( 'NONE',  ( 30.57814311865390167, -3.583136841840119935, -11.00000000000039968 ) ) ;
#21065 = CARTESIAN_POINT ( 'NONE',  ( 35.59419854219520118, 9.774809681453319854, -19.56700000000000017 ) ) ;
#21066 = VERTEX_POINT ( 'NONE', #10499 ) ;
#21067 = CARTESIAN_POINT ( 'NONE',  ( -20.00000000397270128, 22.95208919256889857, -5.499999999995559996 ) ) ;
#21068 = ORIENTED_EDGE ( 'NONE', *, *, #14363, .F. ) ;
#21069 = ORIENTED_EDGE ( 'NONE', *, *, #15600, .T. ) ;
#21070 = CYLINDRICAL_SURFACE ( 'NONE', #1983, 2.067000000000000171 ) ;
#21071 = DIRECTION ( 'NONE',  ( -3.210834492181040124E-17, 2.441916418604790135E-15, 1.000000000000000000 ) ) ;
#21072 = ORIENTED_EDGE ( 'NONE', *, *, #2781, .T. ) ;
#21073 = DIRECTION ( 'NONE',  ( -0.005235963827101446089, 0.9999862922474493931, 5.936218956632777928E-19 ) ) ;
#21074 = AXIS2_PLACEMENT_3D ( 'NONE', #18233, #12542, #3509 ) ;
#21075 = ORIENTED_EDGE ( 'NONE', *, *, #1945, .F. ) ;
#21076 = DIRECTION ( 'NONE',  ( 8.911056267098788616E-18, 1.998401444326210262E-15, 1.000000000000000000 ) ) ;
#21077 = PERSON_AND_ORGANIZATION_ROLE ( 'creator' ) ;
#21078 = DIRECTION ( 'NONE',  ( -1.302733484953870109E-15, -5.237774525740650345E-15, -1.000000000000000000 ) ) ;
#21079 = CALENDAR_DATE ( 2026, 31, 10 ) ;
#21080 = EDGE_CURVE ( 'NONE', #13305, #8538, #6577, .T. ) ;
#21081 = CARTESIAN_POINT ( 'NONE',  ( -29.94170640616770029, 6.343313258985340042, -3.750000000000000000 ) ) ;
#21082 = EDGE_CURVE ( 'NONE', #14758, #13082, #6441, .T. ) ;
#21083 = DIRECTION ( 'NONE',  ( -2.269747459788994803E-13, -2.220446049250330436E-15, -1.000000000000000000 ) ) ;
#21084 = DIRECTION ( 'NONE',  ( 3.099353312215989243E-62, 1.872670541876879671E-92, -1.000000000000000000 ) ) ;
#21085 = ORIENTED_EDGE ( 'NONE', *, *, #13877, .T. ) ;
#21086 = DIRECTION ( 'NONE',  ( -1.138590270679734009E-14, -2.220446049251240387E-15, -1.000000000000000000 ) ) ;
#21087 = AXIS2_PLACEMENT_3D ( 'NONE', #22917, #15799, #23265 ) ;
#21088 = DESIGN_CONTEXT ( 'detailed design', #20535, 'design' ) ;
#21089 = CARTESIAN_POINT ( 'NONE',  ( 37.65360996504041680, 27.78539891644101445, -13.00000000000030020 ) ) ;
#21090 = EDGE_LOOP ( 'NONE', ( #22653, #22754, #7279, #3342, #16286 ) ) ;
#21091 = CARTESIAN_POINT ( 'NONE',  ( 33.59715865393970091, 9.176414746571007086, -8.942923417076592330 ) ) ;
#21092 = DIRECTION ( 'NONE',  ( 3.330999558967088958E-36, 2.805478249480050404E-20, 1.000000000000000000 ) ) ;
#21093 = EDGE_CURVE ( 'NONE', #10552, #20045, #19390, .T. ) ;
#21094 = EDGE_CURVE ( 'NONE', #20134, #5709, #17494, .T. ) ;
#21095 = SECURITY_CLASSIFICATION_LEVEL ( 'unclassified' ) ;
#21096 = CARTESIAN_POINT ( 'NONE',  ( 34.40839383886520153, 23.41606575285519654, -16.27970053837979947 ) ) ;
#21097 = VERTEX_POINT ( 'NONE', #23164 ) ;
#21098 = ORIENTED_EDGE ( 'NONE', *, *, #18381, .F. ) ;
#21099 = PERSON_AND_ORGANIZATION_ROLE ( 'creator' ) ;
#21100 = DIRECTION ( 'NONE',  ( 0.000000000000000000, 2.944971497141790110E-14, -1.000000000000000000 ) ) ;
#21101 = VERTEX_POINT ( 'NONE', #21275 ) ;
#21102 = CIRCLE ( 'NONE', #18852, 3.750000000000001776 ) ;
#21103 = DIRECTION ( 'NONE',  ( -1.187319687680494078E-16, -2.805478249478255076E-20, -1.000000000000000000 ) ) ;
#21104 = PERSON_AND_ORGANIZATION_ROLE ( 'creator' ) ;
#21105 = SECURITY_CLASSIFICATION_LEVEL ( 'unclassified' ) ;
#21106 = FACE_OUTER_BOUND ( 'NONE', #17425, .T. ) ;
#21107 = EDGE_CURVE ( 'NONE', #3684, #20612, #2402, .T. ) ;
#21108 = CARTESIAN_POINT ( 'NONE',  ( 117.1011158151309957, -12.73035498497280038, -20.00000000000000000 ) ) ;
#21109 = VERTEX_POINT ( 'NONE', #1083 ) ;
#21110 = CC_DESIGN_PERSON_AND_ORGANIZATION_ASSIGNMENT ( #30, #3726, ( #6956 ) ) ;
#21111 = VECTOR ( 'NONE', #4573, 1000.000000000000227 ) ;
#21112 = PRODUCT_RELATED_PRODUCT_CATEGORY ( 'detail', '', ( #2832 ) ) ;
#21113 = AXIS2_PLACEMENT_3D ( 'NONE', #9535, #4060, #7985 ) ;
#21114 = ORIENTED_EDGE ( 'NONE', *, *, #19681, .F. ) ;
#21115 = DIRECTION ( 'NONE',  ( -0.005235963827121941846, 0.9999862922474492821, 0.000000000000000000 ) ) ;
#21116 = CARTESIAN_POINT ( 'NONE',  ( 37.67179450110460692, -4.077824265976569329, 13.00000000000000000 ) ) ;
#21117 = ORIENTED_EDGE ( 'NONE', *, *, #4301, .F. ) ;
#21118 = EDGE_CURVE ( 'NONE', #9648, #2588, #9626, .T. ) ;
#21119 = ADVANCED_FACE ( 'NONE', ( #1326 ), #19509, .F. ) ;
#21120 = CARTESIAN_POINT ( 'NONE',  ( 49.97703550743810297, 19.72589006657999988, -13.00000000000049916 ) ) ;
#21121 = DIRECTION ( 'NONE',  ( -1.187319687680494078E-16, -2.805478249478265308E-20, -1.000000000000000000 ) ) ;
#21122 = DIRECTION ( 'NONE',  ( -6.662160722082822564E-09, 1.000000000000000000, -2.523234146875356491E-15 ) ) ;
#21123 = ORIENTED_EDGE ( 'NONE', *, *, #13841, .T. ) ;
#21124 = VERTEX_POINT ( 'NONE', #1442 ) ;
#21125 = CARTESIAN_POINT ( 'NONE',  ( 113.4570673249340018, -28.10438863268850085, -2.700000000000000178 ) ) ;
#21126 = ORIENTED_EDGE ( 'NONE', *, *, #8388, .T. ) ;
#21127 = APPROVAL_DATE_TIME ( #23019, #19543 ) ;
#21128 = EDGE_LOOP ( 'NONE', ( #5912, #11753, #11700, #336 ) ) ;
#21129 = ORIENTED_EDGE ( 'NONE', *, *, #23264, .F. ) ;
#21130 = CARTESIAN_POINT ( 'NONE',  ( -20.00000000397369959, 22.95208919256949898, -3.750000000000059508 ) ) ;
#21131 = AXIS2_PLACEMENT_3D ( 'NONE', #6949, #19289, #13831 ) ;
#21132 = PERSON_AND_ORGANIZATION_ROLE ( 'design_owner' ) ;
#21133 = CIRCLE ( 'NONE', #10923, 5.999999999999999112 ) ;
#21134 = CARTESIAN_POINT ( 'NONE',  ( -30.72441677844210162, -6.660963241697119841, -2.999000000000090260 ) ) ;
#21135 = EDGE_CURVE ( 'NONE', #14881, #12312, #8705, .T. ) ;
#21136 = AXIS2_PLACEMENT_3D ( 'NONE', #18927, #13691, #21055 ) ;
#21137 = DIRECTION ( 'NONE',  ( 0.000000000000000000, 0.000000000000000000, 1.000000000000000000 ) ) ;
#21138 = DIRECTION ( 'NONE',  ( -6.281952996264290168E-17, -4.969341027148640384E-15, -1.000000000000000000 ) ) ;
#21139 = APPROVAL_ROLE ( '' ) ;
#21140 = ORIENTED_EDGE ( 'NONE', *, *, #16872, .F. ) ;
#21141 = CIRCLE ( 'NONE', #9389, 2.499999999999998224 ) ;
#21142 = PLANE ( 'NONE',  #14432 ) ;
#21143 = DIRECTION ( 'NONE',  ( -0.9730401042858036753, 0.2306359803922031493, 5.432877459303543355E-17 ) ) ;
#21144 = VERTEX_POINT ( 'NONE', #8591 ) ;
#21145 = ADVANCED_FACE ( 'NONE', ( #15825 ), #17380, .T. ) ;
#21146 = EDGE_CURVE ( 'NONE', #9786, #8780, #6263, .T. ) ;
#21147 = VECTOR ( 'NONE', #15976, 1000.000000000000114 ) ;
#21148 = CIRCLE ( 'NONE', #18128, 2.066999999999999726 ) ;
#21149 = CARTESIAN_POINT ( 'NONE',  ( 13.68761142428060040, 14.96724437631790039, -3.520083394366879149E-15 ) ) ;
#21151 = AXIS2_PLACEMENT_3D ( 'NONE', #19897, #16434, #23208 ) ;
#21150 = DIRECTION ( 'NONE',  ( -0.7071067811865475727, 1.387778780781445281E-15, 0.7071067811865475727 ) ) ;
#21152 = CARTESIAN_POINT ( 'NONE',  ( -1.262685242559879909E-14, -17.30000000000000071, 2.500000000000000000 ) ) ;
#21153 = VERTEX_POINT ( 'NONE', #8940 ) ;
#21154 = DIRECTION ( 'NONE',  ( -0.1153179901961009640, -0.4865200521429018377, 0.8660254037844385966 ) ) ;
#21155 = APPROVAL_STATUS ( 'not_yet_approved' ) ;
#21156 = EDGE_LOOP ( 'NONE', ( #17285, #13538, #9422, #1152 ) ) ;
#21157 = VERTEX_POINT ( 'NONE', #5364 ) ;
#21158 = DIRECTION ( 'NONE',  ( -0.9730401042858022320, 0.2306359803922080343, 5.959266323858941219E-17 ) ) ;
#21159 = DIRECTION ( 'NONE',  ( 0.9730401042858024541, -0.2306359803922080898, -5.959266323862942222E-17 ) ) ;
#21160 = DIRECTION ( 'NONE',  ( 0.000000000000000000, 1.000000000000000000, 0.000000000000000000 ) ) ;
#21161 = VECTOR ( 'NONE', #5297, 1000.000000000000227 ) ;
#21162 = DATE_AND_TIME ( #5245, #14492 ) ;
#21163 = FACE_OUTER_BOUND ( 'NONE', #168, .T. ) ;
#21164 = CARTESIAN_POINT ( 'NONE',  ( -62.74088165156670271, -25.10566213532069924, -5.538319619822460249E-15 ) ) ;
#21165 = LINE ( 'NONE', #3117, #1797 ) ;
#21166 = EDGE_CURVE ( 'NONE', #23172, #17928, #20078, .T. ) ;
#21167 = AXIS2_PLACEMENT_3D ( 'NONE', #7514, #22211, #16751 ) ;
#21168 = ORIENTED_EDGE ( 'NONE', *, *, #6488, .F. ) ;
#21169 = CARTESIAN_POINT ( 'NONE',  ( 118.6002496876800052, -6.405594307115070052, -15.90000000000000036 ) ) ;
#21170 = APPROVAL_STATUS ( 'not_yet_approved' ) ;
#21171 = DIRECTION ( 'NONE',  ( -1.000000000000000000, 2.775557561562891351E-15, 0.000000000000000000 ) ) ;
#21172 = DIRECTION ( 'NONE',  ( -0.9730401042858035643, 0.2306359803922028717, 5.958148513035547083E-17 ) ) ;
#21173 = EDGE_CURVE ( 'NONE', #467, #22280, #23242, .T. ) ;
#21174 = CARTESIAN_POINT ( 'NONE',  ( -14.98746859791960162, 26.70208920133150343, 6.750000000004400036 ) ) ;
#21175 = PLANE ( 'NONE',  #18969 ) ;
#21176 = EDGE_CURVE ( 'NONE', #9333, #15872, #21965, .T. ) ;
#21177 = DIRECTION ( 'NONE',  ( -3.099353312215988811E-62, 0.000000000000000000, 1.000000000000000000 ) ) ;
#21178 = EDGE_LOOP ( 'NONE', ( #20615, #18910, #7366, #692 ) ) ;
#21179 = DIRECTION ( 'NONE',  ( 0.000000000000000000, 0.000000000000000000, -1.000000000000000000 ) ) ;
#21180 = ORIENTED_EDGE ( 'NONE', *, *, #20816, .F. ) ;
#21181 = EDGE_LOOP ( 'NONE', ( #7702, #6462 ) ) ;
#21182 = LINE ( 'NONE', #1459, #5787 ) ;
#21183 = VECTOR ( 'NONE', #21864, 1000.000000000000227 ) ;
#21184 = DIRECTION ( 'NONE',  ( 1.000000000000000000, 0.000000000000000000, 0.000000000000000000 ) ) ;
#21185 = ORIENTED_EDGE ( 'NONE', *, *, #476, .T. ) ;
#21186 = FACE_OUTER_BOUND ( 'NONE', #13274, .T. ) ;
#21187 = VERTEX_POINT ( 'NONE', #232 ) ;
#21188 = CARTESIAN_POINT ( 'NONE',  ( -17.00058775598304095, -0.04789535763852829919, -3.750000000000000000 ) ) ;
#21189 = APPROVAL_DATE_TIME ( #4572, #18224 ) ;
#21190 = CARTESIAN_POINT ( 'NONE',  ( 35.09747506357100377, 11.43410645592859964, 27.68999999999999773 ) ) ;
#21191 = DATE_TIME_ROLE ( 'classification_date' ) ;
#21192 =( NAMED_UNIT ( * ) PLANE_ANGLE_UNIT ( ) SI_UNIT ( $, .RADIAN. ) );
#21193 = CARTESIAN_POINT ( 'NONE',  ( 0.000000000000000000, 1.250000000000000000, -5.000000000000000000 ) ) ;
#21194 = APPROVAL ( #21437, 'UNSPECIFIED' ) ;
#21195 = DIRECTION ( 'NONE',  ( -0.2306359803922033158, -0.9730401042858034533, 0.000000000000000000 ) ) ;
#21196 =( NAMED_UNIT ( * ) SI_UNIT ( $, .STERADIAN. ) SOLID_ANGLE_UNIT ( ) );
#21197 = CARTESIAN_POINT ( 'NONE',  ( -20.00000000397090005, 22.95208919256900160, 8.250000000004460432 ) ) ;
#21198 = EDGE_LOOP ( 'NONE', ( #940, #1923, #12583, #15447 ) ) ;
#21199 = CARTESIAN_POINT ( 'NONE',  ( -14.00000000397270128, 22.95208919312850071, 6.750000000004400036 ) ) ;
#21200 = DIRECTION ( 'NONE',  ( 0.000000000000000000, 1.000000000000000000, 0.000000000000000000 ) ) ;
#21201 = ORIENTED_EDGE ( 'NONE', *, *, #1275, .F. ) ;
#21202 = CC_DESIGN_APPROVAL ( #17650, ( #18177 ) ) ;
#21203 = CARTESIAN_POINT ( 'NONE',  ( -22.50000000397270128, 22.95208917591822129, 8.000000000004487077 ) ) ;
#21204 = CIRCLE ( 'NONE', #3388, 7.999999999999998224 ) ;
#21205 = DIRECTION ( 'NONE',  ( 1.000000000000000000, -1.187319687680499994E-16, 0.000000000000000000 ) ) ;
#21206 = ORIENTED_EDGE ( 'NONE', *, *, #10518, .T. ) ;
#21207 = SECURITY_CLASSIFICATION_LEVEL ( 'unclassified' ) ;
#21208 = PLANE ( 'NONE',  #6601 ) ;
#21209 = ORIENTED_EDGE ( 'NONE', *, *, #2595, .T. ) ;
#21210 = ORIENTED_EDGE ( 'NONE', *, *, #10150, .T. ) ;
#21211 = CALENDAR_DATE ( 2026, 31, 10 ) ;
#21212 = DIRECTION ( 'NONE',  ( 0.2306359803922080898, 0.9730401042858024541, -2.572202231434325988E-16 ) ) ;
#21213 = ADVANCED_FACE ( 'NONE', ( #16401 ), #1905, .F. ) ;
#21214 = VERTEX_POINT ( 'NONE', #18314 ) ;
#21215 = CYLINDRICAL_SURFACE ( 'NONE', #16584, 3.500000000000000444 ) ;
#21216 = COORDINATED_UNIVERSAL_TIME_OFFSET ( 0, 0, .AHEAD. ) ;
#21217 = PRODUCT ( 'Pin00', 'Pin00', '', ( #17586 ) ) ;
#21218 = CALENDAR_DATE ( 2026, 31, 10 ) ;
#21219 = DIRECTION ( 'NONE',  ( -0.02168293463503252055, 0.9997648975362223300, -2.428612866367530721E-15 ) ) ;
#21220 = AXIS2_PLACEMENT_3D ( 'NONE', #10863, #12509, #3352 ) ;
#21221 = AXIS2_PLACEMENT_3D ( 'NONE', #20198, #337, #15194 ) ;
#21222 = AXIS2_PLACEMENT_3D ( 'NONE', #13479, #15126, #20605 ) ;
#21223 = DIRECTION ( 'NONE',  ( -1.000000000000000000, 2.270069654138870255E-15, 0.000000000000000000 ) ) ;
#21224 = ORIENTED_EDGE ( 'NONE', *, *, #22135, .F. ) ;
#21225 = ORIENTED_EDGE ( 'NONE', *, *, #10435, .F. ) ;
#21226 = DIRECTION ( 'NONE',  ( -0.9730401042858036753, 0.2306359803922028995, 5.959266323858677443E-17 ) ) ;
#21227 = CARTESIAN_POINT ( 'NONE',  ( 40.21613903755276453, 8.679288774590315114, -26.88000000000049283 ) ) ;
#21228 = ORIENTED_EDGE ( 'NONE', *, *, #11732, .T. ) ;
#21229 = LOCAL_TIME ( 14, 11, 27.00000000000000000, #14248 ) ;
#21230 = DIRECTION ( 'NONE',  ( -0.9997651245102238127, -0.02167246670447303680, 0.000000000000000000 ) ) ;
#21231 = DIRECTION ( 'NONE',  ( -3.210834492181045054E-17, 2.441916418604790135E-15, 1.000000000000000000 ) ) ;
#21232 = VERTEX_POINT ( 'NONE', #2039 ) ;
#21233 =( GEOMETRIC_REPRESENTATION_CONTEXT ( 3 ) GLOBAL_UNCERTAINTY_ASSIGNED_CONTEXT ( ( #7525 ) ) GLOBAL_UNIT_ASSIGNED_CONTEXT ( ( #17598, #3567, #23376 ) ) REPRESENTATION_CONTEXT ( 'NONE', 'WORKASPACE' ) );
#21234 = ORIENTED_EDGE ( 'NONE', *, *, #10035, .F. ) ;
#21236 = AXIS2_PLACEMENT_3D ( 'NONE', #4862, #21235, #3078 ) ;
#21235 = DIRECTION ( 'NONE',  ( -2.269747459788990007E-13, -2.220446049250330436E-15, -1.000000000000000000 ) ) ;
#21237 = ORIENTED_EDGE ( 'NONE', *, *, #21094, .T. ) ;
#21238 = APPROVAL_STATUS ( 'not_yet_approved' ) ;
#21239 = ADVANCED_FACE ( 'NONE', ( #1788 ), #7832, .F. ) ;
#21240 = VERTEX_POINT ( 'NONE', #21854 ) ;
#21241 = EDGE_LOOP ( 'NONE', ( #6529, #5048, #12019 ) ) ;
#21242 = LINE ( 'NONE', #14127, #2365 ) ;
#21243 = PERSON_AND_ORGANIZATION_ROLE ( 'creator' ) ;
#21244 = CIRCLE ( 'NONE', #3043, 4.999999999999996447 ) ;
#21245 = CC_DESIGN_DATE_AND_TIME_ASSIGNMENT ( #18274, #16835, ( #8052 ) ) ;
#21246 = CARTESIAN_POINT ( 'NONE',  ( 58.73439644601030096, 17.65016624305009785, -14.25000000000050093 ) ) ;
#21247 = CIRCLE ( 'NONE', #6858, 0.0009999999999225038516 ) ;
#21248 = APPLICATION_CONTEXT ( 'configuration controlled 3d designs of mechanical parts and assemblies' ) ;
#21249 = ADVANCED_FACE ( 'NONE', ( #12958, #9164 ), #19969, .F. ) ;
#21250 = EDGE_CURVE ( 'NONE', #15573, #19560, #610, .T. ) ;
#21251 = LOCAL_TIME ( 14, 11, 27.00000000000000000, #22468 ) ;
#21252 = AXIS2_PLACEMENT_3D ( 'NONE', #9203, #23439, #16097 ) ;
#21253 = DIRECTION ( 'NONE',  ( -2.982858504577314686E-17, 2.441916418604790135E-15, 1.000000000000000000 ) ) ;
#21254 = DATE_AND_TIME ( #14366, #11022 ) ;
#21255 = EDGE_LOOP ( 'NONE', ( #6712, #1401, #16580, #5528 ) ) ;
#21256 = DIRECTION ( 'NONE',  ( -0.9730401042858033422, 0.2306359803922031215, -1.141364251305443211E-16 ) ) ;
#21257 = DIRECTION ( 'NONE',  ( 0.000000000000000000, 0.000000000000000000, 1.000000000000000000 ) ) ;
#21258 = AXIS2_PLACEMENT_3D ( 'NONE', #19841, #18504, #7143 ) ;
#21259 = ORIENTED_EDGE ( 'NONE', *, *, #2005, .F. ) ;
#21260 = DIRECTION ( 'NONE',  ( 0.000000000000000000, 0.000000000000000000, -1.000000000000000000 ) ) ;
#21261 = LINE ( 'NONE', #23150, #15296 ) ;
#21262 = CARTESIAN_POINT ( 'NONE',  ( 114.6071564266699880, -22.31351932764730250, -13.00000000000000000 ) ) ;
#21263 = VERTEX_POINT ( 'NONE', #1678 ) ;
#21264 = FACE_OUTER_BOUND ( 'NONE', #11813, .T. ) ;
#21265 = DATE_AND_TIME ( #4663, #20508 ) ;
#21266 = ADVANCED_FACE ( 'NONE', ( #23400 ), #20209, .T. ) ;
#21267 = CC_DESIGN_APPROVAL ( #11875, ( #10683 ) ) ;
#21268 = ORIENTED_EDGE ( 'NONE', *, *, #8696, .F. ) ;
#21269 = ORIENTED_EDGE ( 'NONE', *, *, #8269, .F. ) ;
#21270 = CARTESIAN_POINT ( 'NONE',  ( 35.59419854219520118, 9.774809681453278998, -26.30000000000050164 ) ) ;
#21271 = FACE_OUTER_BOUND ( 'NONE', #15523, .T. ) ;
#21272 = APPROVAL_PERSON_ORGANIZATION ( #19998, #20397, #14414 ) ;
#21273 = DIRECTION ( 'NONE',  ( -0.9730401042858024541, 0.2306359803922080898, 5.959266323858942451E-17 ) ) ;
#21274 = PERSON_AND_ORGANIZATION ( #11966, #8758 ) ;
#21275 = CARTESIAN_POINT ( 'NONE',  ( 2.499999999999987566, -17.30000000000000782, 2.500000000000000000 ) ) ;
#21276 = CC_DESIGN_PERSON_AND_ORGANIZATION_ASSIGNMENT ( #6035, #9622, ( #8830 ) ) ;
#21277 = AXIS2_PLACEMENT_3D ( 'NONE', #16832, #6265, #17192 ) ;
#21278 = EDGE_LOOP ( 'NONE', ( #11669, #19563, #8886, #6177, #10788, #11854, #6761, #5834, #20058, #14623, #697, #5646 ) ) ;
#21279 = CC_DESIGN_PERSON_AND_ORGANIZATION_ASSIGNMENT ( #20895, #4632, ( #4919 ) ) ;
#21280 = FACE_OUTER_BOUND ( 'NONE', #3758, .T. ) ;
#21281 = ORGANIZATION ( 'NAUO-ORG16', 'UNSPECIFIED', 'UNSPECIFIED' ) ;
#21282 = CARTESIAN_POINT ( 'NONE',  ( -1.614812288830259845, 13.80141363556039913, -4.500000000000000000 ) ) ;
#21283 = VECTOR ( 'NONE', #6624, 1000.000000000000000 ) ;
#21284 = ADVANCED_FACE ( 'NONE', ( #11081 ), #8825, .T. ) ;
#21285 = EDGE_CURVE ( 'NONE', #5959, #19953, #3591, .T. ) ;
#21286 = APPROVAL ( #10032, 'UNSPECIFIED' ) ;
#21287 = DIRECTION ( 'NONE',  ( 0.000000000000000000, 0.000000000000000000, 1.000000000000000000 ) ) ;
#21288 = VERTEX_POINT ( 'NONE', #21507 ) ;
#21289 = CYLINDRICAL_SURFACE ( 'NONE', #4101, 2.500000000000000000 ) ;
#21290 = COORDINATED_UNIVERSAL_TIME_OFFSET ( 0, 0, .AHEAD. ) ;
#21291 = CC_DESIGN_SECURITY_CLASSIFICATION ( #22038, ( #6135 ) ) ;
#21292 = LOCAL_TIME ( 14, 11, 27.00000000000000000, #11450 ) ;
#21293 = CARTESIAN_POINT ( 'NONE',  ( 37.52959221163365555, 9.036526310759173342, 8.996869837679785320 ) ) ;
#21294 = AXIS2_PLACEMENT_3D ( 'NONE', #17796, #14230, #12696 ) ;
#21295 = CARTESIAN_POINT ( 'NONE',  ( -22.49941224781415627, 22.89788185598131420, -2.500000000000039968 ) ) ;
#21296 = LINE ( 'NONE', #22838, #999 ) ;
#21297 = FACE_OUTER_BOUND ( 'NONE', #22289, .T. ) ;
#21298 = EDGE_LOOP ( 'NONE', ( #14503, #22394, #14505 ) ) ;
#21299 = LOCAL_TIME ( 14, 11, 27.00000000000000000, #22514 ) ;
#21300 = CARTESIAN_POINT ( 'NONE',  ( 0.000000000000000000, -1.554450629062379975E-15, 5.000000000000000000 ) ) ;
#21301 = EDGE_CURVE ( 'NONE', #11739, #6720, #10853, .T. ) ;
#21302 = VERTEX_POINT ( 'NONE', #21619 ) ;
#21303 = DIRECTION ( 'NONE',  ( -6.123230199561449365E-17, -4.868008300101910084E-15, -1.000000000000000000 ) ) ;
#21304 = CARTESIAN_POINT ( 'NONE',  ( 0.000000000000000000, 2.220446049250309925E-15, -2.500000000000000000 ) ) ;
#21305 = ORIENTED_EDGE ( 'NONE', *, *, #9343, .F. ) ;
#21306 = DIRECTION ( 'NONE',  ( 0.000000000000000000, 0.000000000000000000, -1.000000000000000000 ) ) ;
#21307 = EDGE_CURVE ( 'NONE', #15573, #18769, #18075, .T. ) ;
#21308 = ORIENTED_EDGE ( 'NONE', *, *, #19019, .T. ) ;
#21309 = CC_DESIGN_APPROVAL ( #22560, ( #3492 ) ) ;
#21310 = LINE ( 'NONE', #14544, #18212 ) ;
#21311 = CALENDAR_DATE ( 2026, 31, 10 ) ;
#21312 = VECTOR ( 'NONE', #5792, 1000.000000000000000 ) ;
#21313 = CARTESIAN_POINT ( 'NONE',  ( -6.134178274321590685, 19.66552749962360025, -1.543041128605420056E-15 ) ) ;
#21314 = EDGE_CURVE ( 'NONE', #17862, #14652, #13144, .T. ) ;
#21315 = EDGE_CURVE ( 'NONE', #4805, #11260, #6708, .T. ) ;
#21316 = VECTOR ( 'NONE', #8982, 1000.000000000000000 ) ;
#21317 = LOCAL_TIME ( 14, 11, 27.00000000000000000, #22878 ) ;
#21318 = CARTESIAN_POINT ( 'NONE',  ( -20.00000000000190070, -20.00000000000000000, -7.999999999995469402 ) ) ;
#21319 = LINE ( 'NONE', #4706, #13209 ) ;
#21320 = DIRECTION ( 'NONE',  ( 0.000000000000000000, 0.000000000000000000, 1.000000000000000000 ) ) ;
#21321 = AXIS2_PLACEMENT_3D ( 'NONE', #16396, #11076, #5359 ) ;
#21322 = DIRECTION ( 'NONE',  ( -3.210834492181045054E-17, 2.441916418604790135E-15, 1.000000000000000000 ) ) ;
#21323 = ORIENTED_EDGE ( 'NONE', *, *, #18904, .T. ) ;
#21324 = CARTESIAN_POINT ( 'NONE',  ( 43.81897180516431689, 0.03336243584794939404, -21.50000000000000000 ) ) ;
#21325 = DESIGN_CONTEXT ( 'detailed design', #21752, 'design' ) ;
#21326 = LOCAL_TIME ( 14, 11, 27.00000000000000000, #4839 ) ;
#21327 = DIRECTION ( 'NONE',  ( -1.466984912809907930E-16, -2.805478249466195144E-20, -1.000000000000000000 ) ) ;
#21328 = ORIENTED_EDGE ( 'NONE', *, *, #12555, .T. ) ;
#21329 = CARTESIAN_POINT ( 'NONE',  ( -25.01253141238650102, 26.70208918381559826, 6.750000000004510170 ) ) ;
#21330 = AXIS2_PLACEMENT_3D ( 'NONE', #10135, #13807, #6562 ) ;
#21331 = DIRECTION ( 'NONE',  ( -0.9999862922474492821, -0.005235963827121953122, 1.239088197126291310E-16 ) ) ;
#21332 = VECTOR ( 'NONE', #2316, 999.9999999999998863 ) ;
#21333 = ORIENTED_EDGE ( 'NONE', *, *, #11180, .T. ) ;
#21334 = APPROVAL_ROLE ( '' ) ;
#21335 = VECTOR ( 'NONE', #12224, 1000.000000000000000 ) ;
#21336 = CYLINDRICAL_SURFACE ( 'NONE', #14929, 0.3999999999999982458 ) ;
#21337 = ORIENTED_EDGE ( 'NONE', *, *, #10098, .F. ) ;
#21338 = EDGE_LOOP ( 'NONE', ( #5258, #4665, #14803, #9728, #8309 ) ) ;
#21339 = DATE_AND_TIME ( #7332, #12216 ) ;
#21340 = CIRCLE ( 'NONE', #14115, 2.499999999999998668 ) ;
#21341 = DIRECTION ( 'NONE',  ( -1.248400535696349791E-16, 3.446306084657144903E-17, 1.000000000000000000 ) ) ;
#21342 = ORIENTED_EDGE ( 'NONE', *, *, #5470, .F. ) ;
#21343 = CARTESIAN_POINT ( 'NONE',  ( -19.99999999999849720, -20.00000000000000000, 6.500000000004389378 ) ) ;
#21344 = AXIS2_PLACEMENT_3D ( 'NONE', #22732, #4705, #22971 ) ;
#21345 = COORDINATED_UNIVERSAL_TIME_OFFSET ( 0, 0, .AHEAD. ) ;
#21346 = AXIS2_PLACEMENT_3D ( 'NONE', #20875, #4615, #9855 ) ;
#21347 = LOCAL_TIME ( 14, 11, 27.00000000000000000, #7302 ) ;
#21348 = CALENDAR_DATE ( 2026, 31, 10 ) ;
#21349 = CARTESIAN_POINT ( 'NONE',  ( -17.50000000000149925, -19.99999998334472195, -6.749999999996036948 ) ) ;
#21350 = AXIS2_PLACEMENT_3D ( 'NONE', #2730, #21018, #6657 ) ;
#21351 = AXIS2_PLACEMENT_3D ( 'NONE', #13462, #852, #8123 ) ;
#21352 = AXIS2_PLACEMENT_3D ( 'NONE', #18246, #20141, #20264 ) ;
#21353 = CARTESIAN_POINT ( 'NONE',  ( -27.00000000000000000, -31.09999999999999787, 2.500000000000000000 ) ) ;
#21354 = VERTEX_POINT ( 'NONE', #13440 ) ;
#21355 = EDGE_CURVE ( 'NONE', #11278, #17959, #14851, .T. ) ;
#21356 = ORIENTED_EDGE ( 'NONE', *, *, #6252, .F. ) ;
#21357 = CIRCLE ( 'NONE', #17570, 5.000000000000001776 ) ;
#21358 = FACE_OUTER_BOUND ( 'NONE', #86, .T. ) ;
#21359 = DIRECTION ( 'NONE',  ( -0.7194962871189606313, -0.6944962871189667153, 0.000000000000000000 ) ) ;
#21360 = ORIENTED_EDGE ( 'NONE', *, *, #9526, .F. ) ;
#21361 = VECTOR ( 'NONE', #23244, 1000.000000000000000 ) ;
#21362 = LOCAL_TIME ( 14, 11, 27.00000000000000000, #2063 ) ;
#21363 = PLANE ( 'NONE',  #21402 ) ;
#21364 = CARTESIAN_POINT ( 'NONE',  ( -19.99995718853209681, 22.95166395734839782, 3.749999999999949818 ) ) ;
#21365 = EDGE_LOOP ( 'NONE', ( #21741, #15660, #9708, #536 ) ) ;
#21366 = ORIENTED_EDGE ( 'NONE', *, *, #11009, .F. ) ;
#21367 = CIRCLE ( 'NONE', #14925, 4.750000000000001776 ) ;
#21368 = EDGE_LOOP ( 'NONE', ( #20308, #10282, #19688, #2554 ) ) ;
#21369 = AXIS2_PLACEMENT_3D ( 'NONE', #13923, #8701, #15929 ) ;
#21370 = CALENDAR_DATE ( 2026, 31, 10 ) ;
#21371 = ORIENTED_EDGE ( 'NONE', *, *, #6971, .F. ) ;
#21372 = VECTOR ( 'NONE', #15467, 1000.000000000000000 ) ;
#21373 = ORIENTED_EDGE ( 'NONE', *, *, #1696, .T. ) ;
#21374 = DIRECTION ( 'NONE',  ( 0.000000000000000000, 0.5102823824563427202, -0.8600069128528436968 ) ) ;
#21375 = PERSON_AND_ORGANIZATION ( #11966, #8758 ) ;
#21376 = LINE ( 'NONE', #8444, #10882 ) ;
#21377 = AXIS2_PLACEMENT_3D ( 'NONE', #23160, #1199, #20924 ) ;
#21378 = AXIS2_PLACEMENT_3D ( 'NONE', #21197, #22973, #6620 ) ;
#21379 = DIRECTION ( 'NONE',  ( -6.662111338785949120E-09, 1.000000000000000000, -1.982541115402066096E-15 ) ) ;
#21380 = CIRCLE ( 'NONE', #21768, 1.000000000000000000 ) ;
#21381 = EDGE_CURVE ( 'NONE', #10115, #17998, #19971, .T. ) ;
#21382 = EDGE_CURVE ( 'NONE', #3813, #11640, #18670, .T. ) ;
#21383 = PERSON_AND_ORGANIZATION ( #11966, #8758 ) ;
#21384 = ORIENTED_EDGE ( 'NONE', *, *, #13856, .F. ) ;
#21385 = CARTESIAN_POINT ( 'NONE',  ( -20.00000000000000000, -20.00000000000000000, 5.000000000004559908 ) ) ;
#21386 = CARTESIAN_POINT ( 'NONE',  ( -17.00003426920497418, -0.08901278465814893570, -2.500000000000000444 ) ) ;
#21387 = VERTEX_POINT ( 'NONE', #14972 ) ;
#21388 = FACE_OUTER_BOUND ( 'NONE', #7492, .T. ) ;
#21389 = CARTESIAN_POINT ( 'NONE',  ( -24.50000000000000000, -28.60000000000000142, 19.00000000000000000 ) ) ;
#21390 = DIRECTION ( 'NONE',  ( 0.2306359803922102825, 0.9730401042858017879, -4.163336342344335449E-15 ) ) ;
#21391 = ORIENTED_EDGE ( 'NONE', *, *, #215, .T. ) ;
#21392 = CARTESIAN_POINT ( 'NONE',  ( -11.25243430249432386, 23.00295828243753249, -3.128898905447639338E-15 ) ) ;
#21393 = EDGE_CURVE ( 'NONE', #11071, #7180, #20670, .T. ) ;
#21394 = EDGE_CURVE ( 'NONE', #11143, #3009, #20728, .T. ) ;
#21395 = PERSON_AND_ORGANIZATION_ROLE ( 'creator' ) ;
#21396 = VECTOR ( 'NONE', #8598, 1000.000000000000000 ) ;
#21397 = ORIENTED_EDGE ( 'NONE', *, *, #13856, .T. ) ;
#21398 = VERTEX_POINT ( 'NONE', #5945 ) ;
#21399 = CARTESIAN_POINT ( 'NONE',  ( 33.27705887009690144, -3.036156860537199798, -13.00000000000039968 ) ) ;
#21400 = DIRECTION ( 'NONE',  ( -0.9730401042858022320, 0.2306359803922080343, 5.959266323858941219E-17 ) ) ;
#21401 = LINE ( 'NONE', #2992, #12959 ) ;
#21402 = AXIS2_PLACEMENT_3D ( 'NONE', #14351, #3550, #23011 ) ;
#21403 = PERSON_AND_ORGANIZATION_ROLE ( 'design_supplier' ) ;
#21404 = CARTESIAN_POINT ( 'NONE',  ( 39.83668191656649782, 5.994421497922120423, -19.59999999999999787 ) ) ;
#21405 = DIRECTION ( 'NONE',  ( 0.000000000000000000, 0.000000000000000000, -1.000000000000000000 ) ) ;
#21406 = DIRECTION ( 'NONE',  ( 1.000000000000000000, 0.000000000000000000, 0.000000000000000000 ) ) ;
#21407 = ORIENTED_EDGE ( 'NONE', *, *, #6344, .T. ) ;
#21408 = CARTESIAN_POINT ( 'NONE',  ( -28.52462712253550237, 6.350733138482030249, -0.7325259402521629992 ) ) ;
#21409 = ADVANCED_FACE ( 'NONE', ( #4048 ), #9519, .T. ) ;
#21410 = DATE_AND_TIME ( #12513, #15224 ) ;
#21411 = CARTESIAN_POINT ( 'NONE',  ( -14.10640258711669937, 21.82649101058139962, 5.000000000000000000 ) ) ;
#21412 = PLANE ( 'NONE',  #7854 ) ;
#21413 = PRODUCT_RELATED_PRODUCT_CATEGORY ( 'detail', '', ( #4576 ) ) ;
#21414 = CARTESIAN_POINT ( 'NONE',  ( -20.00000000000000000, -20.00000000000000000, 5.000000000004559908 ) ) ;
#21415 = LINE ( 'NONE', #2899, #20087 ) ;
#21416 = PRODUCT_RELATED_PRODUCT_CATEGORY ( 'detail', '', ( #11960 ) ) ;
#21417 = PLANE ( 'NONE',  #14484 ) ;
#21418 = VERTEX_POINT ( 'NONE', #22206 ) ;
#21419 = DIRECTION ( 'NONE',  ( 0.9999862922474493931, 0.005235963827108368503, 0.000000000000000000 ) ) ;
#21420 = EDGE_CURVE ( 'NONE', #7235, #3201, #15028, .T. ) ;
#21421 = EDGE_CURVE ( 'NONE', #23217, #17440, #9403, .T. ) ;
#21422 = PRODUCT ( 'Nut', 'Nut', '', ( #1074 ) ) ;
#21423 = ADVANCED_FACE ( 'NONE', ( #4294 ), #9876, .T. ) ;
#21424 = VERTEX_POINT ( 'NONE', #346 ) ;
#21425 = DIRECTION ( 'NONE',  ( -0.04564792618501069266, -0.9989575901083128651, 2.775557561562892534E-15 ) ) ;
#21426 = CARTESIAN_POINT ( 'NONE',  ( -30.15704507771850018, 9.287077397714911697, -2.500000000000000000 ) ) ;
#21427 = EDGE_LOOP ( 'NONE', ( #16576, #17798, #13840, #22216 ) ) ;
#21428 = PLANE ( 'NONE',  #21713 ) ;
#21429 = ORIENTED_EDGE ( 'NONE', *, *, #14709, .F. ) ;
#21430 = CIRCLE ( 'NONE', #4379, 2.500999999999639734 ) ;
#21431 = DIRECTION ( 'NONE',  ( -3.715058581704769953E-16, 5.072287515438380936E-15, 1.000000000000000000 ) ) ;
#21432 = PERSON_AND_ORGANIZATION_ROLE ( 'classification_officer' ) ;
#21433 = DIRECTION ( 'NONE',  ( 0.9730401042858035643, -0.2306359803922028717, 2.740969466505749044E-16 ) ) ;
#21434 = CARTESIAN_POINT ( 'NONE',  ( -29.94170640616770029, 6.343313258985340042, -5.000000000000000000 ) ) ;
#21435 = DIRECTION ( 'NONE',  ( 2.982858504489129897E-17, -2.441916418604790135E-15, -1.000000000000000000 ) ) ;
#21436 = EDGE_CURVE ( 'NONE', #12690, #1957, #13524, .T. ) ;
#21437 = APPROVAL_STATUS ( 'not_yet_approved' ) ;
#21438 = DIRECTION ( 'NONE',  ( -2.269700743865589996E-13, -2.220446049247695246E-15, -1.000000000000000000 ) ) ;
#21439 = APPLICATION_CONTEXT ( 'configuration controlled 3d designs of mechanical parts and assemblies' ) ;
#21440 = VERTEX_POINT ( 'NONE', #18553 ) ;
#21441 = DIRECTION ( 'NONE',  ( 0.4188265566777199522, 0.9080662505684728991, -2.203974058899820124E-15 ) ) ;
#21442 = VECTOR ( 'NONE', #7219, 1000.000000000000114 ) ;
#21443 = DIRECTION ( 'NONE',  ( -0.9999862922474492821, -0.005235963827121953122, 1.466966272682004590E-16 ) ) ;
#21444 = ORIENTED_EDGE ( 'NONE', *, *, #15758, .T. ) ;
#21445 = FACE_OUTER_BOUND ( 'NONE', #22387, .T. ) ;
#21446 = CARTESIAN_POINT ( 'NONE',  ( -20.00479999606039883, 1.846597379377929782, 8.000000000004510170 ) ) ;
#21447 = EDGE_CURVE ( 'NONE', #9763, #1775, #11264, .T. ) ;
#21449 = ORIENTED_EDGE ( 'NONE', *, *, #10530, .T. ) ;
#21448 = ADVANCED_FACE ( 'NONE', ( #13205 ), #20439, .T. ) ;
#21450 = ITEM_DEFINED_TRANSFORMATION ( 'NONE', 'NONE', #10480,  #12739 ) ;
#21451 = CARTESIAN_POINT ( 'NONE',  ( -32.65691263631629226, 9.274125246214069307, 2.500000000000000000 ) ) ;
#21452 = VERTEX_POINT ( 'NONE', #6063 ) ;
#21453 = ORIENTED_EDGE ( 'NONE', *, *, #6070, .F. ) ;
#21454 = CALENDAR_DATE ( 2026, 31, 10 ) ;
#21455 = LINE ( 'NONE', #22884, #17146 ) ;
#21456 = VERTEX_POINT ( 'NONE', #20552 ) ;
#21457 = CARTESIAN_POINT ( 'NONE',  ( -12.93765415188440038, 21.27812940799834962, -3.459521196011834845E-15 ) ) ;
#21458 = APPLICATION_PROTOCOL_DEFINITION ( 'international standard', 'config_control_design', 1994, #8989 ) ;
#21459 = APPROVAL_DATE_TIME ( #7002, #4717 ) ;
#21460 = DIRECTION ( 'NONE',  ( 1.380319151413309694E-18, -2.636191302913840582E-16, 1.000000000000000000 ) ) ;
#21461 = EDGE_CURVE ( 'NONE', #12698, #719, #15800, .T. ) ;
#21462 = DIRECTION ( 'NONE',  ( 0.000000000000000000, -1.000000000000000000, 2.880774829024070580E-15 ) ) ;
#21463 = ORIENTED_EDGE ( 'NONE', *, *, #19668, .F. ) ;
#21464 = ORIENTED_EDGE ( 'NONE', *, *, #12261, .T. ) ;
#21465 = EDGE_CURVE ( 'NONE', #4748, #15533, #2123, .T. ) ;
#21466 = CARTESIAN_POINT ( 'NONE',  ( 5.000000000000000000, -31.09999999999999787, -5.000000000000000000 ) ) ;
#21467 = DIRECTION ( 'NONE',  ( 3.099353312215988811E-62, -1.534091707905539548E-92, -1.000000000000000000 ) ) ;
#21468 = ORIENTED_EDGE ( 'NONE', *, *, #17176, .F. ) ;
#21469 = ADVANCED_FACE ( 'NONE', ( #20284 ), #18269, .F. ) ;
#21470 = VECTOR ( 'NONE', #16619, 1000.000000000000000 ) ;
#21471 = EDGE_CURVE ( 'NONE', #11195, #3145, #10926, .T. ) ;
#21472 = CYLINDRICAL_SURFACE ( 'NONE', #13070, 3.499999999999998668 ) ;
#21473 = CARTESIAN_POINT ( 'NONE',  ( 43.81210844073630284, 9.047859270861110303, -25.00000000000000000 ) ) ;
#21474 = EDGE_LOOP ( 'NONE', ( #18397, #1234, #1168, #2270 ) ) ;
#21475 = ORIENTED_EDGE ( 'NONE', *, *, #10589, .F. ) ;
#21476 = COORDINATED_UNIVERSAL_TIME_OFFSET ( 0, 0, .AHEAD. ) ;
#21477 = EDGE_LOOP ( 'NONE', ( #13046, #23353, #9447, #5579 ) ) ;
#21478 = VERTEX_POINT ( 'NONE', #18033 ) ;
#21479 = CARTESIAN_POINT ( 'NONE',  ( 86.89068504225697609, -33.09999999999999432, -21.50000000000000000 ) ) ;
#21480 = CALENDAR_DATE ( 2026, 31, 10 ) ;
#21481 = DIRECTION ( 'NONE',  ( -0.2306359803922031215, -0.9730401042858035643, 4.741332172907962143E-18 ) ) ;
#21482 = VECTOR ( 'NONE', #10543, 1000.000000000000114 ) ;
#21483 = AXIS2_PLACEMENT_3D ( 'NONE', #6820, #8600, #13829 ) ;
#21484 = VECTOR ( 'NONE', #22594, 1000.000000000000000 ) ;
#21485 = FACE_BOUND ( 'NONE', #17749, .T. ) ;
#21486 = CC_DESIGN_PERSON_AND_ORGANIZATION_ASSIGNMENT ( #14394, #21628, ( #14461 ) ) ;
#21487 = CALENDAR_DATE ( 2026, 31, 10 ) ;
#21488 = VERTEX_POINT ( 'NONE', #18389 ) ;
#21489 = DIRECTION ( 'NONE',  ( -0.9730401042858024541, 0.2306359803922080898, 5.959266323858942451E-17 ) ) ;
#21490 = FACE_OUTER_BOUND ( 'NONE', #5176, .T. ) ;
#21491 = ORIENTED_EDGE ( 'NONE', *, *, #22107, .F. ) ;
#21492 = DIRECTION ( 'NONE',  ( -0.9997651245102240347, -0.02167246670447264822, 0.000000000000000000 ) ) ;
#21493 = CARTESIAN_POINT ( 'NONE',  ( 1.132413798561739802E-13, -1.842903579429180027E-16, -8.889558542813568797E-14 ) ) ;
#21494 = CARTESIAN_POINT ( 'NONE',  ( 0.000000000000000000, 2.499999999999999556, -2.500000000000000000 ) ) ;
#21495 = VECTOR ( 'NONE', #7752, 1000.000000000000114 ) ;
#21496 = EDGE_LOOP ( 'NONE', ( #16428, #1192, #2419, #585 ) ) ;
#21497 = ORIENTED_EDGE ( 'NONE', *, *, #18631, .F. ) ;
#21498 = LINE ( 'NONE', #3339, #16665 ) ;
#21499 = SHAPE_DEFINITION_REPRESENTATION ( #14017, #15964 ) ;
#21500 = EDGE_LOOP ( 'NONE', ( #11556, #7199, #14457 ) ) ;
#21501 = VERTEX_POINT ( 'NONE', #3650 ) ;
#21502 = CARTESIAN_POINT ( 'NONE',  ( -27.00000000000000000, -20.00000000000000000, 5.000000000000000000 ) ) ;
#21503 = DIRECTION ( 'NONE',  ( -0.2306359803922066187, -0.9730401042858026761, 0.000000000000000000 ) ) ;
#21504 = CONICAL_SURFACE ( 'NONE', #11300, 2.254620000000000513, 0.7853981633974461696 ) ;
#21505 = DIRECTION ( 'NONE',  ( 0.2306359803922085339, 0.9730401042858022320, 0.000000000000000000 ) ) ;
#21506 = PERSON_AND_ORGANIZATION ( #11966, #8758 ) ;
#21507 = CARTESIAN_POINT ( 'NONE',  ( 44.14957474989950015, 24.19027144806535290, 19.99999999999975131 ) ) ;
#21508 = EDGE_CURVE ( 'NONE', #16644, #989, #13048, .T. ) ;
#21509 = CARTESIAN_POINT ( 'NONE',  ( 41.15130700480209924, 11.54075009235119964, -15.50000000000000000 ) ) ;
#21510 = VECTOR ( 'NONE', #18217, 1000.000000000000000 ) ;
#21511 = DIRECTION ( 'NONE',  ( 0.000000000000000000, 0.000000000000000000, 1.000000000000000000 ) ) ;
#21512 = VECTOR ( 'NONE', #12490, 1000.000000000000000 ) ;
#21514 = CARTESIAN_POINT ( 'NONE',  ( 102.2474456857739966, -6.023754975411469204, 3.510479034365399954E-14 ) ) ;
#21513 = AXIS2_PLACEMENT_3D ( 'NONE', #1950, #8874, #14205 ) ;
#21515 = PERSON_AND_ORGANIZATION ( #11966, #8758 ) ;
#21516 = CARTESIAN_POINT ( 'NONE',  ( 41.08211621068439712, 11.24883806106539907, 18.89999999999999858 ) ) ;
#21517 = CARTESIAN_POINT ( 'NONE',  ( -26.99999999999959854, -19.33065833018799751, -23.00000000000000000 ) ) ;
#21518 = CARTESIAN_POINT ( 'NONE',  ( 34.40556712239430226, 8.514986143071229918, 28.46999999999999886 ) ) ;
#21519 = DIRECTION ( 'NONE',  ( -2.269700743865584947E-13, -2.220446049247695246E-15, -1.000000000000000000 ) ) ;
#21520 = FACE_OUTER_BOUND ( 'NONE', #9131, .T. ) ;
#21521 = EDGE_LOOP ( 'NONE', ( #8906, #2962 ) ) ;
#21522 = AXIS2_PLACEMENT_3D ( 'NONE', #15877, #14098, #5189 ) ;
#21523 = DIRECTION ( 'NONE',  ( 3.121716675495546285E-31, 4.969341027148640384E-15, 1.000000000000000000 ) ) ;
#21524 = ORIENTED_EDGE ( 'NONE', *, *, #11972, .T. ) ;
#21525 = DIRECTION ( 'NONE',  ( -6.123230199561459225E-17, -4.868008300101910084E-15, -1.000000000000000000 ) ) ;
#21526 = CARTESIAN_POINT ( 'NONE',  ( 35.87511680767496358, 27.43616820587376637, -13.00000000000049916 ) ) ;
#21527 = AXIS2_PLACEMENT_3D ( 'NONE', #8082, #1161, #22905 ) ;
#21528 = ORIENTED_EDGE ( 'NONE', *, *, #19391, .F. ) ;
#21529 = CARTESIAN_POINT ( 'NONE',  ( -19.81505072009858992, 25.44523855881121577, -4.999999999995566213 ) ) ;
#21530 = ADVANCED_FACE ( 'NONE', ( #3886 ), #3544, .T. ) ;
#21531 = ORIENTED_EDGE ( 'NONE', *, *, #11506, .F. ) ;
#21532 = DIRECTION ( 'NONE',  ( -2.471194949999149731E-15, -1.016744709403700171E-14, -1.000000000000000000 ) ) ;
#21533 = CIRCLE ( 'NONE', #1054, 5.000000000000000888 ) ;
#21534 = DATE_TIME_ROLE ( 'classification_date' ) ;
#21535 = CYLINDRICAL_SURFACE ( 'NONE', #5960, 0.4000000000000001887 ) ;
#21536 = CC_DESIGN_DATE_AND_TIME_ASSIGNMENT ( #5270, #12660, ( #20819 ) ) ;
#21537 = CARTESIAN_POINT ( 'NONE',  ( 33.54350891239453603, 19.76716536178353678, 13.00000000000000000 ) ) ;
#21538 = EDGE_CURVE ( 'NONE', #21933, #8196, #19809, .T. ) ;
#21539 = EDGE_CURVE ( 'NONE', #11869, #15046, #7084, .T. ) ;
#21540 = FACE_OUTER_BOUND ( 'NONE', #17129, .T. ) ;
#21541 = DIRECTION ( 'NONE',  ( 1.000000000000000000, 0.000000000000000000, 0.000000000000000000 ) ) ;
#21542 = DIRECTION ( 'NONE',  ( -6.123237831918399306E-17, 1.569224110909209817E-30, 1.000000000000000000 ) ) ;
#21543 = DIRECTION ( 'NONE',  ( 0.2306359803922080898, 0.9730401042858024541, -2.572202231434325988E-16 ) ) ;
#21544 = FACE_OUTER_BOUND ( 'NONE', #20665, .T. ) ;
#21545 = CARTESIAN_POINT ( 'NONE',  ( 37.01481097301077483, 22.79827665208023646, -15.00000000000051159 ) ) ;
#21546 = VECTOR ( 'NONE', #9885, 1000.000000000000114 ) ;
#21547 = ORIENTED_EDGE ( 'NONE', *, *, #21996, .F. ) ;
#21548 = CARTESIAN_POINT ( 'NONE',  ( 0.5364169394695660342, 22.87732758917649889, 4.500000000000000000 ) ) ;
#21549 = DIRECTION ( 'NONE',  ( 2.982858504577324546E-17, -2.441916418604790135E-15, -1.000000000000000000 ) ) ;
#21550 = VERTEX_POINT ( 'NONE', #18150 ) ;
#21551 = DATE_TIME_ROLE ( 'classification_date' ) ;
#21552 = DIRECTION ( 'NONE',  ( 1.224646799147353207E-16, 1.000000000000000000, -0.000000000000000000 ) ) ;
#21553 = ORIENTED_EDGE ( 'NONE', *, *, #816, .T. ) ;
#21554 = EDGE_LOOP ( 'NONE', ( #16081, #13949, #13220, #17775 ) ) ;
#21555 = APPLICATION_CONTEXT ( 'configuration controlled 3d designs of mechanical parts and assemblies' ) ;
#21556 = PERSON_AND_ORGANIZATION_ROLE ( 'classification_officer' ) ;
#21557 = FACE_OUTER_BOUND ( 'NONE', #21090, .T. ) ;
#21558 = EDGE_CURVE ( 'NONE', #8426, #22503, #14269, .T. ) ;
#21559 = VERTEX_POINT ( 'NONE', #21813 ) ;
#21560 = CARTESIAN_POINT ( 'NONE',  ( 118.5079952955230027, -6.794810348829359192, -15.50000000000000000 ) ) ;
#21561 = DATE_AND_TIME ( #8413, #6937 ) ;
#21562 = PRODUCT_RELATED_PRODUCT_CATEGORY ( 'detail', '', ( #8185 ) ) ;
#21564 = CLOSED_SHELL ( 'NONE', ( #949, #11741, #3540, #7778, #16601, #21409, #16176, #12153, #5613, #3054, #7833, #21703, #19574, #12023, #17477, #3654, #2507, #23329 ) ) ;
#21563 = APPROVAL ( #16161, 'UNSPECIFIED' ) ;
#21565 = DATE_AND_TIME ( #9233, #11084 ) ;
#21566 = DIRECTION ( 'NONE',  ( -9.248855984704951398E-11, 1.000000000000000000, 0.000000000000000000 ) ) ;
#21567 = ADVANCED_FACE ( 'NONE', ( #5439 ), #2099, .F. ) ;
#21568 = ADVANCED_FACE ( 'NONE', ( #12695 ), #9349, .T. ) ;
#21569 = SHAPE_REPRESENTATION ( '1602p_c_07', ( #12739 ), #21969 ) ;
#21570 = CARTESIAN_POINT ( 'NONE',  ( -69.90454993788326021, 6.134066389438223688, 5.500000000000099476 ) ) ;
#21571 = VECTOR ( 'NONE', #23124, 1000.000000000000000 ) ;
#21572 = ORIENTED_EDGE ( 'NONE', *, *, #13009, .F. ) ;
#21573 = PLANE ( 'NONE',  #9778 ) ;
#21574 = ORIENTED_EDGE ( 'NONE', *, *, #11271, .T. ) ;
#21575 = FACE_OUTER_BOUND ( 'NONE', #20652, .T. ) ;
#21576 = FACE_OUTER_BOUND ( 'NONE', #18323, .T. ) ;
#21577 = CARTESIAN_POINT ( 'NONE',  ( -17.47493720815199936, 28.95208920939580111, 6.750000000004419576 ) ) ;
#21578 = EDGE_LOOP ( 'NONE', ( #19648, #20806, #9255, #22745 ) ) ;
#21579 = DIRECTION ( 'NONE',  ( -0.9730401042858022320, 0.2306359803922080343, 5.959266323858941219E-17 ) ) ;
#21580 = DIRECTION ( 'NONE',  ( 0.9730401042858036753, -0.2306359803922028995, -5.432877459303547669E-17 ) ) ;
#21581 = EDGE_LOOP ( 'NONE', ( #900, #10468, #1843, #2495 ) ) ;
#21582 = ORIENTED_EDGE ( 'NONE', *, *, #11707, .F. ) ;
#21583 = PERSON_AND_ORGANIZATION ( #11966, #8758 ) ;
#21584 = EDGE_CURVE ( 'NONE', #16270, #6299, #21716, .T. ) ;
#21585 = VERTEX_POINT ( 'NONE', #3759 ) ;
#21586 = ORIENTED_EDGE ( 'NONE', *, *, #2389, .F. ) ;
#21587 = FACE_OUTER_BOUND ( 'NONE', #7224, .T. ) ;
#21588 = APPROVAL_PERSON_ORGANIZATION ( #11296, #17650, #5815 ) ;
#21589 = APPROVAL_ROLE ( '' ) ;
#21590 = CARTESIAN_POINT ( 'NONE',  ( -4.514225866272970400, 4.676725866273559795, -5.000000000000000000 ) ) ;
#21591 = COORDINATED_UNIVERSAL_TIME_OFFSET ( 0, 0, .AHEAD. ) ;
#21592 = EDGE_CURVE ( 'NONE', #16722, #17928, #16467, .T. ) ;
#21593 = EDGE_CURVE ( 'NONE', #19234, #19111, #16241, .T. ) ;
#21594 = LINE ( 'NONE', #12371, #19104 ) ;
#21595 = APPROVAL_DATE_TIME ( #17713, #574 ) ;
#21596 = ORIENTED_EDGE ( 'NONE', *, *, #14511, .F. ) ;
#21597 = AXIS2_PLACEMENT_3D ( 'NONE', #889, #8152, #22728 ) ;
#21598 =( GEOMETRIC_REPRESENTATION_CONTEXT ( 3 ) GLOBAL_UNCERTAINTY_ASSIGNED_CONTEXT ( ( #20741 ) ) GLOBAL_UNIT_ASSIGNED_CONTEXT ( ( #1653, #19595, #12481 ) ) REPRESENTATION_CONTEXT ( 'NONE', 'WORKASPACE' ) );
#21599 = FACE_OUTER_BOUND ( 'NONE', #20441, .T. ) ;
#21600 = VECTOR ( 'NONE', #4038, 1000.000000000000227 ) ;
#21601 = CARTESIAN_POINT ( 'NONE',  ( -62.91331795724000386, 7.826945432762889787, 2.150173005478499992E-15 ) ) ;
#21602 = ORIENTED_EDGE ( 'NONE', *, *, #4721, .F. ) ;
#21603 = CARTESIAN_POINT ( 'NONE',  ( -69.83648240813081998, -6.865755409778319773, 3.000000000000100364 ) ) ;
#21604 = DIRECTION ( 'NONE',  ( 0.000000000000000000, 0.000000000000000000, -1.000000000000000000 ) ) ;
#21605 = DIRECTION ( 'NONE',  ( -0.9730401042858022320, 0.2306359803922080343, 5.959266323858941219E-17 ) ) ;
#21606 = ORIENTED_EDGE ( 'NONE', *, *, #12033, .T. ) ;
#21607 = ORIENTED_EDGE ( 'NONE', *, *, #4879, .F. ) ;
#21608 = DIRECTION ( 'NONE',  ( 0.9730401042858036753, -0.2306359803922031493, 2.740969466505752002E-16 ) ) ;
#21609 = ORIENTED_EDGE ( 'NONE', *, *, #11567, .T. ) ;
#21610 = VECTOR ( 'NONE', #22707, 1000.000000000000000 ) ;
#21611 = PERSON_AND_ORGANIZATION ( #11966, #8758 ) ;
#21612 = ORIENTED_EDGE ( 'NONE', *, *, #3745, .F. ) ;
#21613 = ORIENTED_EDGE ( 'NONE', *, *, #18662, .F. ) ;
#21614 = DIRECTION ( 'NONE',  ( -5.204170427930418759E-14, -1.951563910473906971E-13, -1.000000000000000000 ) ) ;
#21615 = DIRECTION ( 'NONE',  ( 6.124378941433959925E-17, 0.000000000000000000, 1.000000000000000000 ) ) ;
#21616 = DIRECTION ( 'NONE',  ( 1.000000000000000000, 0.000000000000000000, 0.000000000000000000 ) ) ;
#21617 = PERSON_AND_ORGANIZATION ( #11966, #8758 ) ;
#21618 = PRODUCT_RELATED_PRODUCT_CATEGORY ( 'detail', '', ( #10832 ) ) ;
#21619 = CARTESIAN_POINT ( 'NONE',  ( 30.57814311865390167, -3.583136841840119935, -11.00000000000039968 ) ) ;
#21620 = CC_DESIGN_APPROVAL ( #659, ( #3780 ) ) ;
#21621 = DIRECTION ( 'NONE',  ( 0.2306359803922028995, 0.9730401042858036753, -4.730251413307818851E-15 ) ) ;
#21622 = AXIS2_PLACEMENT_3D ( 'NONE', #13963, #5277, #7426 ) ;
#21623 = AXIS2_PLACEMENT_3D ( 'NONE', #12891, #14669, #9452 ) ;
#21624 = DIRECTION ( 'NONE',  ( 1.000000000000000000, 0.000000000000000000, 0.000000000000000000 ) ) ;
#21625 = VECTOR ( 'NONE', #15391, 1000.000000000000000 ) ;
#21626 = ORIENTED_EDGE ( 'NONE', *, *, #8209, .T. ) ;
#21627 = LINE ( 'NONE', #14393, #19663 ) ;
#21628 = PERSON_AND_ORGANIZATION_ROLE ( 'creator' ) ;
#21629 = DIRECTION ( 'NONE',  ( -0.9730401042858022320, 0.2306359803922080343, 5.959266323858941219E-17 ) ) ;
#21630 = CARTESIAN_POINT ( 'NONE',  ( -20.00000000397360012, 22.95208919256889857, -5.000000000000000000 ) ) ;
#21631 = CARTESIAN_POINT ( 'NONE',  ( 34.24686308852899685, 12.59635270528730011, -3.750000000000000000 ) ) ;
#21632 = EDGE_CURVE ( 'NONE', #6522, #18951, #188, .T. ) ;
#21633 = PRODUCT_DEFINITION_FORMATION_WITH_SPECIFIED_SOURCE ( 'ANY', '', #3606, .NOT_KNOWN. ) ;
#21634 = CARTESIAN_POINT ( 'NONE',  ( -65.82123935389580538, 11.86253283145240012, -5.000000000000000000 ) ) ;
#21635 = CARTESIAN_POINT ( 'NONE',  ( 36.11419503630707339, 11.96864536137821666, -10.74538000000051063 ) ) ;
#21636 = CC_DESIGN_APPROVAL ( #18024, ( #7616 ) ) ;
#21637 = ORIENTED_EDGE ( 'NONE', *, *, #10422, .T. ) ;
#21638 = CARTESIAN_POINT ( 'NONE',  ( 35.39416599996382473, 11.83651012589115936, 8.784148981162486436 ) ) ;
#21639 = AXIS2_PLACEMENT_3D ( 'NONE', #19555, #21092, #21205 ) ;
#21640 = LOCAL_TIME ( 14, 11, 27.00000000000000000, #19669 ) ;
#21641 = ORIENTED_EDGE ( 'NONE', *, *, #7670, .F. ) ;
#21642 = CARTESIAN_POINT ( 'NONE',  ( -31.64153798721130428, 6.334539654120280083, 5.000000000000000000 ) ) ;
#21643 = DIRECTION ( 'NONE',  ( 0.9730401042858036753, -0.2306359803922031493, 2.804983810440361760E-16 ) ) ;
#21644 = EDGE_LOOP ( 'NONE', ( #23144, #9382, #12990, #19713 ) ) ;
#21645 = AXIS2_PLACEMENT_3D ( 'NONE', #3167, #12332, #1476 ) ;
#21646 = DIRECTION ( 'NONE',  ( -1.000000000000000000, 0.000000000000000000, 1.187319687680499994E-16 ) ) ;
#21647 = ORIENTED_EDGE ( 'NONE', *, *, #4148, .F. ) ;
#21648 = CYLINDRICAL_SURFACE ( 'NONE', #19714, 3.000000000000001332 ) ;
#21649 = APPLICATION_PROTOCOL_DEFINITION ( 'international standard', 'config_control_design', 1994, #21439 ) ;
#21650 = LINE ( 'NONE', #10421, #12799 ) ;
#21651 = CC_DESIGN_APPROVAL ( #10713, ( #12572 ) ) ;
#21652 = APPROVAL_PERSON_ORGANIZATION ( #19284, #1159, #4683 ) ;
#21653 = FACE_OUTER_BOUND ( 'NONE', #21496, .T. ) ;
#21654 = DIRECTION ( 'NONE',  ( 0.9730401042858036753, -0.2306359803922031493, 2.740969466505752002E-16 ) ) ;
#21655 = APPROVAL_PERSON_ORGANIZATION ( #442, #1502, #4610 ) ;
#21656 = CARTESIAN_POINT ( 'NONE',  ( -20.00000000000000000, -20.00000000000000000, 0.000000000000000000 ) ) ;
#21657 = DIRECTION ( 'NONE',  ( 0.000000000000000000, 0.000000000000000000, -1.000000000000000000 ) ) ;
#21658 = DIRECTION ( 'NONE',  ( -6.123230174520380038E-17, -4.962644601432250805E-15, -1.000000000000000000 ) ) ;
#21659 = EDGE_CURVE ( 'NONE', #2641, #18216, #20340, .T. ) ;
#21660 = DIRECTION ( 'NONE',  ( -3.099353312215988811E-62, 1.001855809244433740E-92, 1.000000000000000000 ) ) ;
#21661 = EDGE_LOOP ( 'NONE', ( #150, #7580 ) ) ;
#21662 = CARTESIAN_POINT ( 'NONE',  ( 35.34171762861030430, 30.38879166913060104, 15.99999999999969802 ) ) ;
#21663 = DIRECTION ( 'NONE',  ( 0.1982893547227720377, 0.8365715274351381847, 0.5107146084541409614 ) ) ;
#21664 = CC_DESIGN_DATE_AND_TIME_ASSIGNMENT ( #19193, #11848, ( #19794 ) ) ;
#21665 = ORIENTED_EDGE ( 'NONE', *, *, #11082, .T. ) ;
#21666 = CC_DESIGN_APPROVAL ( #20093, ( #9939 ) ) ;
#21667 = CARTESIAN_POINT ( 'NONE',  ( 37.13840842239409312, 23.31972727237329579, 11.00000000000000178 ) ) ;
#21668 = DIRECTION ( 'NONE',  ( 9.249330715586770885E-11, -1.000000000000000000, 2.220446028256680454E-15 ) ) ;
#21669 = ORIENTED_EDGE ( 'NONE', *, *, #1670, .F. ) ;
#21670 = AXIS2_PLACEMENT_3D ( 'NONE', #12576, #7010, #12462 ) ;
#21671 = ADVANCED_FACE ( 'NONE', ( #21575 ), #5312, .F. ) ;
#21672 = ADVANCED_FACE ( 'NONE', ( #7925 ), #4424, .F. ) ;
#21673 = PERSON_AND_ORGANIZATION_ROLE ( 'design_owner' ) ;
#21674 = PLANE ( 'NONE',  #11887 ) ;
#21675 = ORIENTED_EDGE ( 'NONE', *, *, #8768, .F. ) ;
#21676 = CARTESIAN_POINT ( 'NONE',  ( -26.26776695296636888, -31.09999999999999787, -20.76776695296636888 ) ) ;
#21677 = APPROVAL_PERSON_ORGANIZATION ( #11971, #6606, #6365 ) ;
#21678 = DATE_AND_TIME ( #1617, #3897 ) ;
#21679 = DIRECTION ( 'NONE',  ( -6.123230174520380038E-17, -4.962644601432250805E-15, -1.000000000000000000 ) ) ;
#21680 = CC_DESIGN_APPROVAL ( #13443, ( #10349 ) ) ;
#21681 = CARTESIAN_POINT ( 'NONE',  ( 5.000000000000000000, -31.09999999999999787, -6.250000000000000000 ) ) ;
#21682 = VECTOR ( 'NONE', #5377, 999.9999999999998863 ) ;
#21683 = EDGE_LOOP ( 'NONE', ( #8453, #18159, #665, #7230, #22312 ) ) ;
#21684 = DIRECTION ( 'NONE',  ( -3.210834492194344756E-17, 2.441916418604790135E-15, 1.000000000000000000 ) ) ;
#21685 = AXIS2_PLACEMENT_3D ( 'NONE', #11525, #15160, #2824 ) ;
#21686 = EDGE_CURVE ( 'NONE', #17206, #22023, #6377, .T. ) ;
#21687 = VECTOR ( 'NONE', #22636, 1000.000000000000114 ) ;
#21688 = CIRCLE ( 'NONE', #20571, 2.500000000000001332 ) ;
#21689 = ORIENTED_EDGE ( 'NONE', *, *, #6640, .F. ) ;
#21690 = APPROVAL_PERSON_ORGANIZATION ( #15049, #3685, #16701 ) ;
#21691 = DIRECTION ( 'NONE',  ( 2.920245690604589998E-14, 1.234618914536939803E-13, -1.000000000000000000 ) ) ;
#21692 = PLANE ( 'NONE',  #10321 ) ;
#21693 = DIRECTION ( 'NONE',  ( 0.005235963827108352890, -0.9999862922474493931, -5.936218956694023463E-19 ) ) ;
#21694 = ORIENTED_EDGE ( 'NONE', *, *, #2327, .T. ) ;
#21695 = APPLICATION_CONTEXT ( 'configuration controlled 3d designs of mechanical parts and assemblies' ) ;
#21696 = PRODUCT_RELATED_PRODUCT_CATEGORY ( 'detail', '', ( #7796 ) ) ;
#21697 = AXIS2_PLACEMENT_3D ( 'NONE', #13221, #845, #15345 ) ;
#21698 = CC_DESIGN_DATE_AND_TIME_ASSIGNMENT ( #10815, #12470, ( #4578 ) ) ;
#21699 = DIRECTION ( 'NONE',  ( 4.063875459488300452E-16, -1.011971878839181895E-16, -1.000000000000000000 ) ) ;
#21700 = DIRECTION ( 'NONE',  ( -0.005235963827117092427, 0.9999862922474493931, 2.636227439667000721E-16 ) ) ;
#21701 = ORIENTED_EDGE ( 'NONE', *, *, #9406, .F. ) ;
#21702 = EDGE_CURVE ( 'NONE', #10449, #418, #4440, .T. ) ;
#21703 = ADVANCED_FACE ( 'NONE', ( #552 ), #11859, .T. ) ;
#21704 = COORDINATED_UNIVERSAL_TIME_OFFSET ( 0, 0, .AHEAD. ) ;
#21705 = APPROVAL_PERSON_ORGANIZATION ( #19941, #4013, #3560 ) ;
#21706 = ORIENTED_EDGE ( 'NONE', *, *, #23468, .F. ) ;
#21707 = ORIENTED_EDGE ( 'NONE', *, *, #7121, .T. ) ;
#21708 = CC_DESIGN_PERSON_AND_ORGANIZATION_ASSIGNMENT ( #16851, #9496, ( #3780 ) ) ;
#21709 = DIRECTION ( 'NONE',  ( 2.269747459789000104E-13, 2.220446049250330436E-15, 1.000000000000000000 ) ) ;
#21710 = CALENDAR_DATE ( 2026, 31, 10 ) ;
#21711 = AXIS2_PLACEMENT_3D ( 'NONE', #3450, #8926, #12725 ) ;
#21712 = CIRCLE ( 'NONE', #22851, 2.066999999999997950 ) ;
#21713 = AXIS2_PLACEMENT_3D ( 'NONE', #3369, #17867, #10640 ) ;
#21714 = FACE_OUTER_BOUND ( 'NONE', #360, .T. ) ;
#21715 = DATE_AND_TIME ( #1757, #15530 ) ;
#21716 =( BOUNDED_CURVE ( )  B_SPLINE_CURVE ( 2, ( #19928, #2217, #9471 ),
 .UNSPECIFIED., .F., .F. ) 
 B_SPLINE_CURVE_WITH_KNOTS ( ( 3, 3 ),
 ( 0.1168436138077860315, 0.2336872276155859962 ),
 .UNSPECIFIED. ) 
 CURVE ( )  GEOMETRIC_REPRESENTATION_ITEM ( )  RATIONAL_B_SPLINE_CURVE ( ( 1.077350269189624843, 1.077350269189629506, 1.000000000000000000 ) ) 
 REPRESENTATION_ITEM ( '' )  );
#21717 = LINE ( 'NONE', #99, #13097 ) ;
#21718 = VECTOR ( 'NONE', #11958, 999.9999999999998863 ) ;
#21719 =( NAMED_UNIT ( * ) PLANE_ANGLE_UNIT ( ) SI_UNIT ( $, .RADIAN. ) );
#21721 = CONICAL_SURFACE ( 'NONE', #14516, 2.729132938682640397, 1.047197551196598297 ) ;
#21720 = CARTESIAN_POINT ( 'NONE',  ( 5.000000000000000000, -23.36217782649100272, -5.000000000000000000 ) ) ;
#21722 = AXIS2_PLACEMENT_3D ( 'NONE', #6394, #4382, #11650 ) ;
#21723 = PERSON_AND_ORGANIZATION_ROLE ( 'design_owner' ) ;
#21724 = EDGE_CURVE ( 'NONE', #16163, #12545, #19097, .T. ) ;
#21725 = CC_DESIGN_SECURITY_CLASSIFICATION ( #5063, ( #17948 ) ) ;
#21726 = VERTEX_POINT ( 'NONE', #2340 ) ;
#21727 = CIRCLE ( 'NONE', #2002, 2.499999999999998668 ) ;
#21728 = CARTESIAN_POINT ( 'NONE',  ( 39.27359436029389883, 22.26288585089444894, 12.99999999999979927 ) ) ;
#21729 = ORIENTED_EDGE ( 'NONE', *, *, #8486, .T. ) ;
#21730 = AXIS2_PLACEMENT_3D ( 'NONE', #1078, #15579, #21048 ) ;
#21731 = EDGE_CURVE ( 'NONE', #17474, #4562, #5566, .T. ) ;
#21732 = CYLINDRICAL_SURFACE ( 'NONE', #4470, 5.000000000000000888 ) ;
#21733 = DIRECTION ( 'NONE',  ( -0.005235963827117092427, 0.9999862922474493931, 2.636227439667000721E-16 ) ) ;
#21734 = DIRECTION ( 'NONE',  ( 0.2306359803922080343, 0.9730401042858022320, -2.539064864905560527E-14 ) ) ;
#21735 = ORIENTED_EDGE ( 'NONE', *, *, #10864, .T. ) ;
#21736 = ORIENTED_EDGE ( 'NONE', *, *, #5841, .F. ) ;
#21737 = CARTESIAN_POINT ( 'NONE',  ( 27.87922736721089834, -4.130116823143030302, -13.00000000000039968 ) ) ;
#21738 = EDGE_LOOP ( 'NONE', ( #9154, #12520, #5012, #16158 ) ) ;
#21739 = EDGE_CURVE ( 'NONE', #6317, #23250, #666, .T. ) ;
#21740 = DATE_AND_TIME ( #12617, #3056 ) ;
#21742 = ADVANCED_FACE ( 'NONE', ( #22524 ), #8164, .T. ) ;
#21741 = ORIENTED_EDGE ( 'NONE', *, *, #18127, .F. ) ;
#21743 = VERTEX_POINT ( 'NONE', #15393 ) ;
#21744 = DIRECTION ( 'NONE',  ( 2.269747459789000104E-13, 2.220446049250330436E-15, 1.000000000000000000 ) ) ;
#21745 = AXIS2_PLACEMENT_3D ( 'NONE', #9436, #16654, #4335 ) ;
#21746 = CARTESIAN_POINT ( 'NONE',  ( 39.83668191656649782, 5.994421497922090225, -18.89999999999999858 ) ) ;
#21747 = PERSON_AND_ORGANIZATION ( #11966, #8758 ) ;
#21748 = CARTESIAN_POINT ( 'NONE',  ( 43.45766680872284837, 21.27115113520779843, -13.00000000000030020 ) ) ;
#21749 = APPROVAL_PERSON_ORGANIZATION ( #8730, #1801, #3615 ) ;
#21750 = VECTOR ( 'NONE', #22035, 1000.000000000000000 ) ;
#21751 = CARTESIAN_POINT ( 'NONE',  ( -26.00000000397469790, 22.95208919201850151, -7.999999999994199307 ) ) ;
#21752 = APPLICATION_CONTEXT ( 'configuration controlled 3d designs of mechanical parts and assemblies' ) ;
#21753 = AXIS2_PLACEMENT_3D ( 'NONE', #17366, #16914, #7896 ) ;
#21754 = AXIS2_PLACEMENT_3D ( 'NONE', #20042, #14942, #22169 ) ;
#21755 = DIRECTION ( 'NONE',  ( 1.000000000000000000, 0.000000000000000000, 0.000000000000000000 ) ) ;
#21756 = EDGE_LOOP ( 'NONE', ( #2984, #18942, #7353, #13392 ) ) ;
#21757 = CARTESIAN_POINT ( 'NONE',  ( 32.14184541509679605, -2.767081550079510510, 13.00000000000019895 ) ) ;
#21758 = COORDINATED_UNIVERSAL_TIME_OFFSET ( 0, 0, .AHEAD. ) ;
#21759 = CARTESIAN_POINT ( 'NONE',  ( -26.99999999999959854, -19.33065833018799751, 25.00000000000000000 ) ) ;
#21760 = CARTESIAN_POINT ( 'NONE',  ( 13.08336378532089839, 15.11046688687759776, -3.694269929671379468E-15 ) ) ;
#21761 = CARTESIAN_POINT ( 'NONE',  ( 36.78282996199610722, 11.03463321983559986, -29.25000000000050093 ) ) ;
#21762 = EDGE_CURVE ( 'NONE', #19270, #15831, #5187, .T. ) ;
#21763 = VECTOR ( 'NONE', #1716, 1000.000000000000000 ) ;
#21764 = DIRECTION ( 'NONE',  ( -0.9997651245102161521, -0.02167246670483388357, 0.000000000000000000 ) ) ;
#21765 = EDGE_CURVE ( 'NONE', #21109, #2277, #6020, .T. ) ;
#21766 = CYLINDRICAL_SURFACE ( 'NONE', #6536, 2.500000000028978597 ) ;
#21767 = VERTEX_POINT ( 'NONE', #11634 ) ;
#21768 = AXIS2_PLACEMENT_3D ( 'NONE', #6175, #13428, #22779 ) ;
#21769 = CARTESIAN_POINT ( 'NONE',  ( 33.51035039627143419, 9.711136848494149376, 8.987168322345956639 ) ) ;
#21770 = UNCERTAINTY_MEASURE_WITH_UNIT (LENGTH_MEASURE( 1.000000000000000082E-05 ), #6478, 'distance_accuracy_value', 'NONE');
#21771 = EDGE_CURVE ( 'NONE', #12554, #4733, #9606, .T. ) ;
#21772 = ORIENTED_EDGE ( 'NONE', *, *, #20238, .T. ) ;
#21773 = CARTESIAN_POINT ( 'NONE',  ( -19.99999998648642574, 20.45208919256890212, -7.999999999995544009 ) ) ;
#21774 = PLANE ( 'NONE',  #11760 ) ;
#21775 = VERTEX_POINT ( 'NONE', #11520 ) ;
#21776 = DIRECTION ( 'NONE',  ( -0.2306359803922028995, -0.9730401042858035643, -1.064172857958375654E-32 ) ) ;
#21777 = VERTEX_POINT ( 'NONE', #18861 ) ;
#21778 = CARTESIAN_POINT ( 'NONE',  ( -19.99999998564990022, 20.20208919256900160, 8.500000000004467537 ) ) ;
#21779 = APPROVAL_DATE_TIME ( #14545, #1801 ) ;
#21780 = DIRECTION ( 'NONE',  ( 0.000000000000000000, 0.000000000000000000, 1.000000000000000000 ) ) ;
#21781 = DIRECTION ( 'NONE',  ( 0.9730401042858036753, -0.2306359803922028995, 2.740969466505749537E-16 ) ) ;
#21782 = DIRECTION ( 'NONE',  ( -2.269747459788994803E-13, -2.220446049250320181E-15, -1.000000000000000000 ) ) ;
#21783 = COORDINATED_UNIVERSAL_TIME_OFFSET ( 0, 0, .AHEAD. ) ;
#21784 = CARTESIAN_POINT ( 'NONE',  ( -16.00004797695752856, -0.08377682083102051813, -1.143293334710289765E-14 ) ) ;
#21785 = DIRECTION ( 'NONE',  ( -0.9730401042858036753, 0.2306359803922028995, 5.959266323858677443E-17 ) ) ;
#21786 = SPHERICAL_SURFACE ( 'NONE', #9328, 15.25000000000000000 ) ;
#21787 = DESIGN_CONTEXT ( 'detailed design', #22188, 'design' ) ;
#21788 = PLANE ( 'NONE',  #18258 ) ;
#21789 = LINE ( 'NONE', #16323, #8498 ) ;
#21790 = DIRECTION ( 'NONE',  ( -0.9999862922464065607, -0.005235964026270698360, -1.932211826555549481E-17 ) ) ;
#21791 = ORIENTED_EDGE ( 'NONE', *, *, #19391, .T. ) ;
#21792 = VERTEX_POINT ( 'NONE', #14935 ) ;
#21793 = FACE_OUTER_BOUND ( 'NONE', #11371, .T. ) ;
#21794 = CARTESIAN_POINT ( 'NONE',  ( 35.34171762861030430, 30.38879166913060104, 19.99999999999969802 ) ) ;
#21795 = EDGE_LOOP ( 'NONE', ( #12015, #10581 ) ) ;
#21796 = VECTOR ( 'NONE', #3183, 1000.000000000000114 ) ;
#21797 = PERSON_AND_ORGANIZATION_ROLE ( 'design_supplier' ) ;
#21798 = CARTESIAN_POINT ( 'NONE',  ( 6.500000000000000000, -17.30000000000000071, -2.500000000000000000 ) ) ;
#21799 = ORIENTED_EDGE ( 'NONE', *, *, #12586, .F. ) ;
#21800 = DIRECTION ( 'NONE',  ( -0.2306359803922087282, -0.9730401042858021210, 5.204170427930421283E-15 ) ) ;
#21801 = DATE_AND_TIME ( #12899, #103 ) ;
#21802 = ADVANCED_FACE ( 'NONE', ( #22278 ), #22164, .T. ) ;
#21803 = EDGE_CURVE ( 'NONE', #13888, #14120, #2582, .T. ) ;
#21804 = COORDINATED_UNIVERSAL_TIME_OFFSET ( 0, 0, .AHEAD. ) ;
#21805 = CARTESIAN_POINT ( 'NONE',  ( 45.07211867146970263, 28.08243186520990164, 13.00000000000000000 ) ) ;
#21806 = ADVANCED_BREP_SHAPE_REPRESENTATION ( '', ( #9531, #12739 ), #2093 ) ;
#21807 = CIRCLE ( 'NONE', #10473, 2.499999999999999112 ) ;
#21808 = CARTESIAN_POINT ( 'NONE',  ( -19.49999999982360066, -0.1021026942259579962, 5.000000000000000000 ) ) ;
#21809 = EDGE_LOOP ( 'NONE', ( #16124, #10314, #9817, #8121 ) ) ;
#21810 = DIRECTION ( 'NONE',  ( -0.9730401042858022320, 0.2306359803922080343, 5.959266323858941219E-17 ) ) ;
#21811 = EDGE_CURVE ( 'NONE', #11532, #3079, #5907, .T. ) ;
#21812 = EDGE_LOOP ( 'NONE', ( #16226, #20190, #17848, #9281, #3942 ) ) ;
#21813 = CARTESIAN_POINT ( 'NONE',  ( 115.3944095602285387, -19.93085175668762332, 13.00000000000000000 ) ) ;
#21814 = DIRECTION ( 'NONE',  ( -0.005235963827121952255, 0.9999862922474493931, -2.738476122049126182E-14 ) ) ;
#21815 = PLANE ( 'NONE',  #19224 ) ;
#21816 = EDGE_LOOP ( 'NONE', ( #18479, #4071, #910, #14671 ) ) ;
#21817 = CALENDAR_DATE ( 2026, 31, 10 ) ;
#21818 = LINE ( 'NONE', #5800, #3497 ) ;
#21819 = EDGE_LOOP ( 'NONE', ( #19498, #15232, #20886, #4778 ) ) ;
#21820 = SHAPE_DEFINITION_REPRESENTATION ( #13836, #4456 ) ;
#21821 = ORIENTED_EDGE ( 'NONE', *, *, #8865, .T. ) ;
#21822 = VECTOR ( 'NONE', #21460, 1000.000000000000000 ) ;
#21823 = EDGE_LOOP ( 'NONE', ( #17482, #788 ) ) ;
#21824 = CARTESIAN_POINT ( 'NONE',  ( -20.00000000397270128, 22.95208919256889857, -4.999999999995559996 ) ) ;
#21825 = PERSON_AND_ORGANIZATION ( #11966, #8758 ) ;
#21826 = VECTOR ( 'NONE', #16100, 1000.000000000000227 ) ;
#21827 = EDGE_CURVE ( 'NONE', #13418, #18259, #18088, .T. ) ;
#21828 = CARTESIAN_POINT ( 'NONE',  ( 5.000000000000000000, -31.09999999999999787, -19.00000000000000000 ) ) ;
#21829 = LINE ( 'NONE', #16488, #14979 ) ;
#21830 = CC_DESIGN_DATE_AND_TIME_ASSIGNMENT ( #5978, #19591, ( #5821 ) ) ;
#21831 = CC_DESIGN_PERSON_AND_ORGANIZATION_ASSIGNMENT ( #21506, #6575, ( #11475 ) ) ;
#21832 =( NAMED_UNIT ( * ) SI_UNIT ( $, .STERADIAN. ) SOLID_ANGLE_UNIT ( ) );
#21833 = DIRECTION ( 'NONE',  ( 0.4999931461237248076, 0.002617981913554119633, 0.8660254037844385966 ) ) ;
#21834 = EDGE_CURVE ( 'NONE', #7554, #12280, #21058, .T. ) ;
#21835 = ADVANCED_FACE ( 'NONE', ( #21445 ), #2929, .F. ) ;
#21836 = SHAPE_DEFINITION_REPRESENTATION ( #8541, #19781 ) ;
#21837 =( GEOMETRIC_REPRESENTATION_CONTEXT ( 3 ) GLOBAL_UNCERTAINTY_ASSIGNED_CONTEXT ( ( #19638 ) ) GLOBAL_UNIT_ASSIGNED_CONTEXT ( ( #6700, #15242, #8242 ) ) REPRESENTATION_CONTEXT ( 'NONE', 'WORKASPACE' ) );
#21838 = VERTEX_POINT ( 'NONE', #6739 ) ;
#21839 = CARTESIAN_POINT ( 'NONE',  ( 118.4388045014059969, -7.086722380115130449, 19.59999999999999787 ) ) ;
#21840 = ORIENTED_EDGE ( 'NONE', *, *, #9544, .T. ) ;
#21841 = FACE_OUTER_BOUND ( 'NONE', #3076, .T. ) ;
#21842 = CARTESIAN_POINT ( 'NONE',  ( -19.99975861755300244, 22.95209442650120124, 2.499999999999900524 ) ) ;
#21843 = ORIENTED_EDGE ( 'NONE', *, *, #313, .T. ) ;
#21844 = ORIENTED_EDGE ( 'NONE', *, *, #1763, .F. ) ;
#21845 = CARTESIAN_POINT ( 'NONE',  ( 29.87858131747766421, 2.137125494442494222, 13.00000000000019895 ) ) ;
#21846 = ORIENTED_EDGE ( 'NONE', *, *, #2508, .T. ) ;
#21847 = APPROVAL_ROLE ( '' ) ;
#21848 = ORIENTED_EDGE ( 'NONE', *, *, #8939, .F. ) ;
#21849 = EDGE_LOOP ( 'NONE', ( #2574, #1486, #12729 ) ) ;
#21850 = DIRECTION ( 'NONE',  ( 2.269881297312570136E-47, 1.000000000000000000, -2.269881297312570136E-47 ) ) ;
#21851 =( BOUNDED_CURVE ( )  B_SPLINE_CURVE ( 2, ( #14974, #4167, #21857 ),
 .UNSPECIFIED., .F., .F. ) 
 B_SPLINE_CURVE_WITH_KNOTS ( ( 3, 3 ),
 ( 0.1168436138077977582, 0.2336872276155859962 ),
 .UNSPECIFIED. ) 
 CURVE ( )  GEOMETRIC_REPRESENTATION_ITEM ( )  RATIONAL_B_SPLINE_CURVE ( ( 1.077350269189629950, 1.077350269189626841, 1.000000000000000000 ) ) 
 REPRESENTATION_ITEM ( '' )  );
#21852 = DIRECTION ( 'NONE',  ( 0.8660135325225012393, 0.004534477687579934260, -0.4999999999999995004 ) ) ;
#21853 = APPROVAL_ROLE ( '' ) ;
#21854 = CARTESIAN_POINT ( 'NONE',  ( -25.65326162860803194, 22.49081825942809942, -2.500000000000000888 ) ) ;
#21855 = ADVANCED_FACE ( 'NONE', ( #17540 ), #21869, .T. ) ;
#21856 = VECTOR ( 'NONE', #7397, 1000.000000000000000 ) ;
#21857 = CARTESIAN_POINT ( 'NONE',  ( 36.57467860885130051, 21.71590586959139912, 11.00000000000000000 ) ) ;
#21858 = CIRCLE ( 'NONE', #15412, 2.499999999999998224 ) ;
#21859 = APPROVAL ( #2141, 'UNSPECIFIED' ) ;
#21860 = APPROVAL ( #15322, 'UNSPECIFIED' ) ;
#21861 = EDGE_CURVE ( 'NONE', #23222, #20392, #7477, .T. ) ;
#21862 = EDGE_CURVE ( 'NONE', #5829, #2485, #4826, .T. ) ;
#21863 = VERTEX_POINT ( 'NONE', #23218 ) ;
#21864 = DIRECTION ( 'NONE',  ( 0.4999931461237239749, 0.002617981913554110092, -0.8660254037844389297 ) ) ;
#21865 = CALENDAR_DATE ( 2026, 31, 10 ) ;
#21866 = VERTEX_POINT ( 'NONE', #12099 ) ;
#21867 = FACE_OUTER_BOUND ( 'NONE', #21812, .T. ) ;
#21868 = DIRECTION ( 'NONE',  ( 0.9822637906114334294, -0.1875042550281410536, 4.933538860811975815E-16 ) ) ;
#21869 = TOROIDAL_SURFACE ( 'NONE', #20743, 2.380000000000000338, 2.370000000000000107 ) ;
#21870 = CARTESIAN_POINT ( 'NONE',  ( 39.76749112244880280, 5.702509466636339397, 15.50000000000000000 ) ) ;
#21871 = AXIS2_PLACEMENT_3D ( 'NONE', #17630, #2786, #15481 ) ;
#21872 = DIRECTION ( 'NONE',  ( 6.124378941434239724E-17, -2.274246353359159970E-33, 1.000000000000000000 ) ) ;
#21873 = VERTEX_POINT ( 'NONE', #21203 ) ;
#21874 = CARTESIAN_POINT ( 'NONE',  ( 34.60161846897012339, 7.941814927679100578, 8.772741540512809522 ) ) ;
#21875 = ORIENTED_EDGE ( 'NONE', *, *, #5469, .T. ) ;
#21876 = CARTESIAN_POINT ( 'NONE',  ( -26.00000000000179767, -20.00000000055539928, -6.749999999994109601 ) ) ;
#21877 = CARTESIAN_POINT ( 'NONE',  ( -13.66075527208050033, 1.277470069177119916, -3.750000000000000000 ) ) ;
#21878 = AXIS2_PLACEMENT_3D ( 'NONE', #16647, #12992, #7764 ) ;
#21879 = ORIENTED_EDGE ( 'NONE', *, *, #21659, .T. ) ;
#21880 = DIRECTION ( 'NONE',  ( 0.9730401042858036753, -0.2306359803922031493, 2.740969466505752002E-16 ) ) ;
#21882 = ORIENTED_EDGE ( 'NONE', *, *, #4735, .F. ) ;
#21881 = EDGE_CURVE ( 'NONE', #10063, #11032, #10440, .T. ) ;
#21883 = LINE ( 'NONE', #4078, #258 ) ;
#21884 = AXIS2_PLACEMENT_3D ( 'NONE', #23066, #10279, #17396 ) ;
#21885 = CONTEXT_DEPENDENT_SHAPE_REPRESENTATION ( #23403, #14796 ) ;
#21886 = DIRECTION ( 'NONE',  ( 0.9730401042858035643, -0.2306359803922028717, -5.959266323858667582E-17 ) ) ;
#21887 = AXIS2_PLACEMENT_3D ( 'NONE', #19803, #2688, #15277 ) ;
#21888 = ADVANCED_FACE ( 'NONE', ( #19554 ), #1366, .T. ) ;
#21889 = VECTOR ( 'NONE', #514, 1000.000000000000000 ) ;
#21890 = VECTOR ( 'NONE', #9145, 1000.000000000000000 ) ;
#21891 = SHAPE_REPRESENTATION_RELATIONSHIP ( 'NONE' , 'NONE' ,  #13540, #14455 ) ;
#21892 = DIRECTION ( 'NONE',  ( -0.7070970883417637687, -0.003702385528188433840, 0.7071067811865477948 ) ) ;
#21893 = EDGE_CURVE ( 'NONE', #17965, #3931, #22746, .T. ) ;
#21894 = CARTESIAN_POINT ( 'NONE',  ( -19.99975861755289941, 22.95209442650110176, 2.499999999999950262 ) ) ;
#21895 = DIRECTION ( 'NONE',  ( 0.000000000000000000, 0.000000000000000000, 1.000000000000000000 ) ) ;
#21896 = EDGE_CURVE ( 'NONE', #4600, #12280, #19203, .T. ) ;
#21897 = CARTESIAN_POINT ( 'NONE',  ( -25.44839750738890061, 25.46504853262630164, -5.000000000000070166 ) ) ;
#21898 = CARTESIAN_POINT ( 'NONE',  ( 36.10037903421270755, -9.768828191507928693, -2.700000000000000178 ) ) ;
#21899 = CARTESIAN_POINT ( 'NONE',  ( -65.80336369117380002, 8.448563927732790191, 5.000000000000000000 ) ) ;
#21900 = FACE_OUTER_BOUND ( 'NONE', #18267, .T. ) ;
#21901 = AXIS2_PLACEMENT_3D ( 'NONE', #5574, #12608, #19848 ) ;
#21902 = DIRECTION ( 'NONE',  ( -0.9730401042858035643, 0.2306359803922028717, 6.126766849694256332E-17 ) ) ;
#21903 = CARTESIAN_POINT ( 'NONE',  ( -69.82862846239015653, -8.365734848149525504, 7.200000000000000178 ) ) ;
#21904 = ORIENTED_EDGE ( 'NONE', *, *, #9988, .T. ) ;
#21905 = AXIS2_PLACEMENT_3D ( 'NONE', #14425, #21543, #21657 ) ;
#21906 = ORIENTED_EDGE ( 'NONE', *, *, #980, .F. ) ;
#21907 = CARTESIAN_POINT ( 'NONE',  ( 33.87576285740820481, 21.16892588828840260, -13.00000000000049916 ) ) ;
#21908 = AXIS2_PLACEMENT_3D ( 'NONE', #18715, #2301, #2181 ) ;
#21909 = LINE ( 'NONE', #14565, #1148 ) ;
#21910 = ORIENTED_EDGE ( 'NONE', *, *, #4023, .T. ) ;
#21911 = CARTESIAN_POINT ( 'NONE',  ( 31.37708959083939675, -0.2124270449897310287, 13.00000000000019895 ) ) ;
#21912 = ORIENTED_EDGE ( 'NONE', *, *, #23415, .F. ) ;
#21913 = CARTESIAN_POINT ( 'NONE',  ( 35.11747397072451804, 7.763535785894566388, -19.56699999999998951 ) ) ;
#21914 = DATE_AND_TIME ( #12447, #11899 ) ;
#21915 = CARTESIAN_POINT ( 'NONE',  ( 35.65846783274012211, 7.691313958534617967, -8.772741540512798863 ) ) ;
#21916 = CC_DESIGN_PERSON_AND_ORGANIZATION_ASSIGNMENT ( #23300, #12634, ( #20770 ) ) ;
#21917 = COORDINATED_UNIVERSAL_TIME_OFFSET ( 0, 0, .AHEAD. ) ;
#21918 = AXIS2_PLACEMENT_3D ( 'NONE', #13382, #6255, #18614 ) ;
#21919 = DIRECTION ( 'NONE',  ( -0.9999862922464843873, -0.005235964011397749134, 0.000000000000000000 ) ) ;
#21920 = ORIENTED_EDGE ( 'NONE', *, *, #2082, .T. ) ;
#21921 = VECTOR ( 'NONE', #7744, 1000.000000000000000 ) ;
#21922 = DIRECTION ( 'NONE',  ( 3.099353312215989243E-62, 1.872670541876879671E-92, -1.000000000000000000 ) ) ;
#21923 = ORIENTED_EDGE ( 'NONE', *, *, #12310, .T. ) ;
#21924 = CARTESIAN_POINT ( 'NONE',  ( -69.87051617300704720, -0.3658445101694126067, 0.000000000000000000 ) ) ;
#21925 = ORIENTED_EDGE ( 'NONE', *, *, #14417, .T. ) ;
#21926 = DIRECTION ( 'NONE',  ( 1.541924204231519956E-16, 1.400987035803820065E-18, -1.000000000000000000 ) ) ;
#21927 = CARTESIAN_POINT ( 'NONE',  ( 33.27705887009660302, -3.036156860536630031, -13.00000000000000000 ) ) ;
#21928 = ORIENTED_EDGE ( 'NONE', *, *, #1764, .T. ) ;
#21929 = EDGE_CURVE ( 'NONE', #22384, #22900, #6852, .T. ) ;
#21930 = DIRECTION ( 'NONE',  ( 1.213490492418610097E-15, 4.861311874477940294E-15, 1.000000000000000000 ) ) ;
#21931 = ORIENTED_EDGE ( 'NONE', *, *, #11213, .F. ) ;
#21932 = CALENDAR_DATE ( 2026, 31, 10 ) ;
#21933 = VERTEX_POINT ( 'NONE', #17773 ) ;
#21934 = ORIENTED_EDGE ( 'NONE', *, *, #4769, .T. ) ;
#21935 = CARTESIAN_POINT ( 'NONE',  ( 38.22140682376687693, 9.152092534394331125, -26.30000000000049809 ) ) ;
#21936 = CIRCLE ( 'NONE', #10595, 6.499999999999997335 ) ;
#21937 = PERSON_AND_ORGANIZATION_ROLE ( 'design_supplier' ) ;
#21938 = CARTESIAN_POINT ( 'NONE',  ( 114.9405074087380001, 12.84085624101770051, 2.915350241847199977E-14 ) ) ;
#21939 = DATE_TIME_ROLE ( 'classification_date' ) ;
#21940 = DIRECTION ( 'NONE',  ( 0.000000000000000000, 1.734723475976806848E-16, 1.000000000000000000 ) ) ;
#21941 =( NAMED_UNIT ( * ) PLANE_ANGLE_UNIT ( ) SI_UNIT ( $, .RADIAN. ) );
#21942 = DIRECTION ( 'NONE',  ( -0.2306359803922080343, -0.9730401042858022320, -7.611545645951921999E-14 ) ) ;
#21943 = APPROVAL_ROLE ( '' ) ;
#21944 = ORIENTED_EDGE ( 'NONE', *, *, #23132, .T. ) ;
#21945 = DIRECTION ( 'NONE',  ( 1.000000000000000000, 9.248967332749676061E-11, -1.142026288351397951E-14 ) ) ;
#21946 = ORIENTED_EDGE ( 'NONE', *, *, #22013, .F. ) ;
#21947 = EDGE_CURVE ( 'NONE', #2112, #9304, #5946, .T. ) ;
#21948 = DIRECTION ( 'NONE',  ( 0.000000000000000000, 0.000000000000000000, -1.000000000000000000 ) ) ;
#21949 = CARTESIAN_POINT ( 'NONE',  ( -20.00000000397400157, 22.95208919257349933, -5.499999999995569766 ) ) ;
#21950 = DIRECTION ( 'NONE',  ( -2.269700743865584947E-13, -2.220446049247695246E-15, -1.000000000000000000 ) ) ;
#21951 = ORIENTED_EDGE ( 'NONE', *, *, #3993, .T. ) ;
#21952 = LOCAL_TIME ( 14, 11, 27.00000000000000000, #16027 ) ;
#21953 = ORIENTED_EDGE ( 'NONE', *, *, #4069, .T. ) ;
#21955 = DIRECTION ( 'NONE',  ( -3.099353312215989243E-62, 1.534091707905539548E-92, 1.000000000000000000 ) ) ;
#21954 = CIRCLE ( 'NONE', #5285, 3.750000000000000000 ) ;
#21956 = VERTEX_POINT ( 'NONE', #6009 ) ;
#21957 = APPROVAL ( #10675, 'UNKNOWN' ) ;
#21958 = PERSON_AND_ORGANIZATION_ROLE ( 'design_owner' ) ;
#21959 = ORIENTED_EDGE ( 'NONE', *, *, #13106, .F. ) ;
#21960 = EDGE_LOOP ( 'NONE', ( #15902, #16039, #4057, #19417 ) ) ;
#21961 = DIRECTION ( 'NONE',  ( 0.7806762821593211665, -0.6249356306643909509, -7.632783294297951215E-15 ) ) ;
#21962 = DIRECTION ( 'NONE',  ( 0.000000000000000000, -0.9999588795606764169, -0.009068582455730644573 ) ) ;
#21963 = APPLICATION_PROTOCOL_DEFINITION ( 'international standard', 'config_control_design', 1994, #4574 ) ;
#21964 = EDGE_CURVE ( 'NONE', #7019, #15512, #15815, .T. ) ;
#21965 = LINE ( 'NONE', #7276, #22223 ) ;
#21966 = EDGE_CURVE ( 'NONE', #17265, #13085, #13253, .T. ) ;
#21967 = CARTESIAN_POINT ( 'NONE',  ( 39.27359436029429673, 22.26288585089420025, -13.00000000000049916 ) ) ;
#21968 = AXIS2_PLACEMENT_3D ( 'NONE', #22258, #4106, #11374 ) ;
#21969 =( GEOMETRIC_REPRESENTATION_CONTEXT ( 3 ) GLOBAL_UNCERTAINTY_ASSIGNED_CONTEXT ( ( #6266 ) ) GLOBAL_UNIT_ASSIGNED_CONTEXT ( ( #13093, #2262, #9882 ) ) REPRESENTATION_CONTEXT ( 'NONE', 'WORKASPACE' ) );
#21970 = VECTOR ( 'NONE', #12124, 1000.000000000000000 ) ;
#21971 = ORIENTED_EDGE ( 'NONE', *, *, #17621, .F. ) ;
#21972 = FACE_OUTER_BOUND ( 'NONE', #12072, .T. ) ;
#21973 = APPROVAL_STATUS ( 'not_yet_approved' ) ;
#21974 = ORIENTED_EDGE ( 'NONE', *, *, #18961, .T. ) ;
#21976 = DIRECTION ( 'NONE',  ( -6.123237831918399306E-17, 1.569224110909209817E-30, 1.000000000000000000 ) ) ;
#21975 = VECTOR ( 'NONE', #4689, 1000.000000000000227 ) ;
#21977 = DIRECTION ( 'NONE',  ( -0.9999862922474492821, -0.005235963827121953122, 1.466966272682004590E-16 ) ) ;
#21978 = DIRECTION ( 'NONE',  ( 4.906471675765221317E-19, -0.9999862926232440108, -0.005235892055781489474 ) ) ;
#21979 = ADVANCED_FACE ( 'NONE', ( #4228 ), #7910, .T. ) ;
#21980 = CARTESIAN_POINT ( 'NONE',  ( -68.70795112897079093, 11.84741790582710053, 3.773156417642989929E-15 ) ) ;
#21981 =( BOUNDED_CURVE ( )  B_SPLINE_CURVE ( 2, ( #21899, #12881, #20126 ),
 .UNSPECIFIED., .F., .F. ) 
 B_SPLINE_CURVE_WITH_KNOTS ( ( 3, 3 ),
 ( 0.000000000000000000, 0.5842180690389598974 ),
 .UNSPECIFIED. ) 
 CURVE ( )  GEOMETRIC_REPRESENTATION_ITEM ( )  RATIONAL_B_SPLINE_CURVE ( ( 1.000000000000000000, 1.154700538379249908, 1.000000000000000000 ) ) 
 REPRESENTATION_ITEM ( '' )  );
#21982 = CYLINDRICAL_SURFACE ( 'NONE', #12994, 0.0009999999999615351298 ) ;
#21983 = VERTEX_POINT ( 'NONE', #2203 ) ;
#21984 = FACE_OUTER_BOUND ( 'NONE', #15869, .T. ) ;
#21985 = UNCERTAINTY_MEASURE_WITH_UNIT (LENGTH_MEASURE( 1.000000000000000082E-05 ), #11409, 'distance_accuracy_value', 'NONE');
#21986 = APPROVAL ( #2804, 'UNSPECIFIED' ) ;
#21987 = PRODUCT_DEFINITION_SHAPE ( 'NONE', 'NONE',  #23511 ) ;
#21988 = CC_DESIGN_APPROVAL ( #15773, ( #6843 ) ) ;
#21989 = ORIENTED_EDGE ( 'NONE', *, *, #8856, .T. ) ;
#21990 = CC_DESIGN_PERSON_AND_ORGANIZATION_ASSIGNMENT ( #8753, #17894, ( #16369 ) ) ;
#21991 = ORIENTED_EDGE ( 'NONE', *, *, #15494, .T. ) ;
#21992 = DIRECTION ( 'NONE',  ( -2.269747459788994803E-13, -2.220446049250470459E-15, -1.000000000000000000 ) ) ;
#21993 = DIRECTION ( 'NONE',  ( -0.9730401042858035643, 0.2306359803922028717, 5.959266323858679908E-17 ) ) ;
#21994 = EDGE_LOOP ( 'NONE', ( #17929, #9746, #5936, #3612 ) ) ;
#21995 = EDGE_CURVE ( 'NONE', #11195, #13864, #10911, .T. ) ;
#21996 = EDGE_CURVE ( 'NONE', #15512, #12945, #15026, .T. ) ;
#21997 = VERTEX_POINT ( 'NONE', #20379 ) ;
#21998 = PRODUCT_RELATED_PRODUCT_CATEGORY ( 'detail', '', ( #5117 ) ) ;
#21999 = CARTESIAN_POINT ( 'NONE',  ( 4.267766952966340455, -28.60000000000000497, 20.76776695296636532 ) ) ;
#22000 = COORDINATED_UNIVERSAL_TIME_OFFSET ( 0, 0, .AHEAD. ) ;
#22001 = CARTESIAN_POINT ( 'NONE',  ( -22.52506283708579815, 28.95208917575130414, 6.750000000004479972 ) ) ;
#22002 = CIRCLE ( 'NONE', #11797, 1.250000000000000222 ) ;
#22003 = VECTOR ( 'NONE', #19510, 1000.000000000000114 ) ;
#22004 = APPLICATION_CONTEXT ( 'configuration controlled 3d designs of mechanical parts and assemblies' ) ;
#22005 = FACE_OUTER_BOUND ( 'NONE', #21024, .T. ) ;
#22006 = CARTESIAN_POINT ( 'NONE',  ( 34.88044566782589584, 28.44271146055899990, 17.99999999999970157 ) ) ;
#22007 = APPROVAL_DATE_TIME ( #7651, #1881 ) ;
#22008 = PRODUCT_DEFINITION_FORMATION_WITH_SPECIFIED_SOURCE ( 'ANY', '', #12523, .NOT_KNOWN. ) ;
#22009 = APPROVAL_PERSON_ORGANIZATION ( #5680, #7944, #7831 ) ;
#22010 = DIRECTION ( 'NONE',  ( 0.000000000000000000, -1.000000000000000000, 5.551115123125781913E-15 ) ) ;
#22011 = DIRECTION ( 'NONE',  ( 0.000000000000000000, 0.000000000000000000, -1.000000000000000000 ) ) ;
#22012 = DIRECTION ( 'NONE',  ( -0.2306359803922010121, -0.9730401042858040084, 0.000000000000000000 ) ) ;
#22013 = EDGE_CURVE ( 'NONE', #8304, #21585, #16945, .T. ) ;
#22014 = CARTESIAN_POINT ( 'NONE',  ( 36.57467860885130051, 21.71590586959130320, -15.00000000000049916 ) ) ;
#22015 = LINE ( 'NONE', #14664, #17975 ) ;
#22016 = PLANE ( 'NONE',  #11499 ) ;
#22017 = AXIS2_PLACEMENT_3D ( 'NONE', #7031, #21489, #8920 ) ;
#22018 = VERTEX_POINT ( 'NONE', #4108 ) ;
#22019 = EDGE_CURVE ( 'NONE', #746, #3635, #13543, .T. ) ;
#22020 = VERTEX_POINT ( 'NONE', #2457 ) ;
#22021 = DIRECTION ( 'NONE',  ( -0.9730401042858035643, 0.2306359803922028717, 5.958148513035547083E-17 ) ) ;
#22022 = CARTESIAN_POINT ( 'NONE',  ( -14.00000000202680006, 1.899127378930359988, -5.499999999996879829 ) ) ;
#22023 = VERTEX_POINT ( 'NONE', #650 ) ;
#22024 = EDGE_CURVE ( 'NONE', #12280, #7554, #8317, .T. ) ;
#22025 = CARTESIAN_POINT ( 'NONE',  ( 36.78282996199610722, 11.03463321983590006, 27.68999999999999773 ) ) ;
#22026 = ORIENTED_EDGE ( 'NONE', *, *, #21593, .F. ) ;
#22027 = APPROVAL_PERSON_ORGANIZATION ( #18041, #9379, #14473 ) ;
#22028 = EDGE_CURVE ( 'NONE', #1281, #22077, #20147, .T. ) ;
#22029 = CARTESIAN_POINT ( 'NONE',  ( 11.50000000000000000, -23.36217782649110219, -5.000000000000000000 ) ) ;
#22030 = LOCAL_TIME ( 14, 11, 27.00000000000000000, #7401 ) ;
#22031 = DATE_TIME_ROLE ( 'creation_date' ) ;
#22032 = DIRECTION ( 'NONE',  ( 0.9999862922474493931, 0.005235963827116132258, -1.187304881134280213E-16 ) ) ;
#22033 = ORGANIZATION ( 'NAUO-ORG20', 'UNSPECIFIED', 'UNSPECIFIED' ) ;
#22034 = ORIENTED_EDGE ( 'NONE', *, *, #22160, .T. ) ;
#22035 = DIRECTION ( 'NONE',  ( 0.000000000000000000, 0.000000000000000000, -1.000000000000000000 ) ) ;
#22036 = ORIENTED_EDGE ( 'NONE', *, *, #5872, .F. ) ;
#22037 = DIRECTION ( 'NONE',  ( 2.269747459789000104E-13, 2.220446049250330436E-15, 1.000000000000000000 ) ) ;
#22038 = SECURITY_CLASSIFICATION ( '', '', #15465 ) ;
#22039 = LINE ( 'NONE', #23380, #11428 ) ;
#22040 = ORIENTED_EDGE ( 'NONE', *, *, #9478, .F. ) ;
#22041 = CARTESIAN_POINT ( 'NONE',  ( -27.39120887301850260, 6.327965799971420502, 5.000000000000000000 ) ) ;
#22042 = CARTESIAN_POINT ( 'NONE',  ( 114.8905747189831033, 12.63019305843987361, -2.067000000000024595 ) ) ;
#22043 = CYLINDRICAL_SURFACE ( 'NONE', #12046, 2.499999999999998224 ) ;
#22044 = ORIENTED_EDGE ( 'NONE', *, *, #22553, .T. ) ;
#22045 = AXIS2_PLACEMENT_3D ( 'NONE', #10497, #21273, #21505 ) ;
#22046 = DATE_AND_TIME ( #307, #16765 ) ;
#22047 = CARTESIAN_POINT ( 'NONE',  ( -19.99975861755300244, 22.95209442650120124, 3.749999999999900080 ) ) ;
#22048 = EDGE_CURVE ( 'NONE', #18753, #5830, #293, .T. ) ;
#22049 = APPROVAL_PERSON_ORGANIZATION ( #16929, #18067, #14922 ) ;
#22050 = ORIENTED_EDGE ( 'NONE', *, *, #20292, .F. ) ;
#22051 = DATE_AND_TIME ( #14817, #3457 ) ;
#22052 = CYLINDRICAL_SURFACE ( 'NONE', #16761, 2.500000000000001776 ) ;
#22053 = ORIENTED_EDGE ( 'NONE', *, *, #7330, .T. ) ;
#22054 = ORIENTED_EDGE ( 'NONE', *, *, #19813, .F. ) ;
#22055 = DIRECTION ( 'NONE',  ( 0.000000000000000000, 0.000000000000000000, -1.000000000000000000 ) ) ;
#22056 = COORDINATED_UNIVERSAL_TIME_OFFSET ( 0, 0, .AHEAD. ) ;
#22057 = CC_DESIGN_APPROVAL ( #10684, ( #5761 ) ) ;
#22058 = CARTESIAN_POINT ( 'NONE',  ( 122.7747609327790030, 11.20643158045800014, 9.133960000000000079 ) ) ;
#22059 = ITEM_DEFINED_TRANSFORMATION ( 'NONE', 'NONE', #376,  #12739 ) ;
#22060 = DIRECTION ( 'NONE',  ( 0.000000000000000000, 0.000000000000000000, 1.000000000000000000 ) ) ;
#22061 = AXIS2_PLACEMENT_3D ( 'NONE', #3709, #5257, #12519 ) ;
#22062 = EDGE_CURVE ( 'NONE', #4119, #23217, #8154, .T. ) ;
#22063 = VECTOR ( 'NONE', #20864, 1000.000000000000000 ) ;
#22064 = CONICAL_SURFACE ( 'NONE', #7306, 2.283500000000000085, 0.7853981633974447263 ) ;
#22065 = SECURITY_CLASSIFICATION ( '', '', #20288 ) ;
#22066 = DIRECTION ( 'NONE',  ( 2.982858504577319616E-17, -2.441916418604790135E-15, -1.000000000000000000 ) ) ;
#22067 = AXIS2_PLACEMENT_3D ( 'NONE', #1695, #21523, #5259 ) ;
#22068 = COORDINATED_UNIVERSAL_TIME_OFFSET ( 0, 0, .AHEAD. ) ;
#22069 = VECTOR ( 'NONE', #3588, 999.9999999999998863 ) ;
#22070 = ORIENTED_EDGE ( 'NONE', *, *, #17621, .T. ) ;
#22071 = DIRECTION ( 'NONE',  ( -4.028143194477080210E-16, -2.054129435991050111E-15, -1.000000000000000000 ) ) ;
#22072 = ORIENTED_EDGE ( 'NONE', *, *, #13020, .F. ) ;
#22073 = LOCAL_TIME ( 14, 11, 27.00000000000000000, #20178 ) ;
#22074 = CYLINDRICAL_SURFACE ( 'NONE', #14317, 2.500000000000000444 ) ;
#22075 = CARTESIAN_POINT ( 'NONE',  ( -30.79177721110609767, 6.338862259904598950, -2.999707106781159816 ) ) ;
#22076 = PLANE ( 'NONE',  #12266 ) ;
#22077 = VERTEX_POINT ( 'NONE', #15740 ) ;
#22078 = VERTEX_POINT ( 'NONE', #12084 ) ;
#22079 = FACE_OUTER_BOUND ( 'NONE', #1105, .T. ) ;
#22080 = CIRCLE ( 'NONE', #15260, 3.499999999999998668 ) ;
#22081 = ORIENTED_EDGE ( 'NONE', *, *, #15006, .F. ) ;
#22082 = VECTOR ( 'NONE', #4921, 1000.000000000000000 ) ;
#22083 = APPROVAL_ROLE ( '' ) ;
#22084 = VERTEX_POINT ( 'NONE', #10181 ) ;
#22085 = CIRCLE ( 'NONE', #23224, 2.501000000000000334 ) ;
#22086 = VERTEX_POINT ( 'NONE', #2677 ) ;
#22087 = DIRECTION ( 'NONE',  ( 0.000000000000000000, 0.000000000000000000, 1.000000000000000000 ) ) ;
#22088 = LINE ( 'NONE', #5361, #18018 ) ;
#22089 = DATE_AND_TIME ( #18313, #4634 ) ;
#22090 = DIRECTION ( 'NONE',  ( 2.269747459788990007E-13, 2.220446049250330436E-15, 1.000000000000000000 ) ) ;
#22091 = AXIS2_PLACEMENT_3D ( 'NONE', #19637, #4916, #12183 ) ;
#22092 = CARTESIAN_POINT ( 'NONE',  ( -23.49893655333865894, 22.87624079303418156, 5.000000000000000000 ) ) ;
#22093 = AXIS2_PLACEMENT_3D ( 'NONE', #10819, #5558, #9132 ) ;
#22094 = EDGE_CURVE ( 'NONE', #20342, #15812, #22611, .T. ) ;
#22095 = CIRCLE ( 'NONE', #6954, 1.000000000000000000 ) ;
#22096 = EDGE_CURVE ( 'NONE', #10096, #18339, #1391, .T. ) ;
#22097 = LOCAL_TIME ( 14, 11, 27.00000000000000000, #13603 ) ;
#22098 = AXIS2_PLACEMENT_3D ( 'NONE', #14352, #12361, #19581 ) ;
#22099 = VERTEX_POINT ( 'NONE', #2805 ) ;
#22100 = ADVANCED_BREP_SHAPE_REPRESENTATION ( '', ( #9329, #12739 ), #16529 ) ;
#22101 = DIRECTION ( 'NONE',  ( -0.9730401042858036753, 0.2306359803922031493, 5.432877459303543355E-17 ) ) ;
#22102 = PERSON_AND_ORGANIZATION_ROLE ( 'design_owner' ) ;
#22103 = CONICAL_SURFACE ( 'NONE', #16042, 5.086751345948125724, 1.047197551196598297 ) ;
#22104 = EDGE_LOOP ( 'NONE', ( #8552, #16252, #7783, #6431 ) ) ;
#22105 = CARTESIAN_POINT ( 'NONE',  ( 62.70840910389689782, 3.348031886875269869, 1.061114750357439988E-14 ) ) ;
#22106 = CARTESIAN_POINT ( 'NONE',  ( 28.94448933012489888, 0.3641629059907759425, 13.00000000000019895 ) ) ;
#22107 = EDGE_CURVE ( 'NONE', #16045, #18419, #6724, .T. ) ;
#22108 = EDGE_CURVE ( 'NONE', #14944, #8200, #3025, .T. ) ;
#22109 = CARTESIAN_POINT ( 'NONE',  ( 36.79228697538940196, -6.849707878650439952, 3.399999999999999911 ) ) ;
#22110 = DIRECTION ( 'NONE',  ( 0.000000000000000000, -1.000000000000000000, 2.081668171172169697E-15 ) ) ;
#22111 = ORIENTED_EDGE ( 'NONE', *, *, #14549, .F. ) ;
#22112 = VECTOR ( 'NONE', #4817, 1000.000000000000000 ) ;
#22113 = DIRECTION ( 'NONE',  ( 0.000000000000000000, 0.000000000000000000, 1.000000000000000000 ) ) ;
#22114 = SECURITY_CLASSIFICATION ( '', '', #18218 ) ;
#22115 = CIRCLE ( 'NONE', #893, 0.1000000000000028644 ) ;
#22116 = ORIENTED_EDGE ( 'NONE', *, *, #20816, .T. ) ;
#22117 = EDGE_LOOP ( 'NONE', ( #20896, #15443, #8027, #1839 ) ) ;
#22118 = DIRECTION ( 'NONE',  ( 3.210834492194360164E-17, -2.441916418604790135E-15, -1.000000000000000000 ) ) ;
#22119 = LINE ( 'NONE', #20808, #20837 ) ;
#22120 = ORIENTED_EDGE ( 'NONE', *, *, #15900, .F. ) ;
#22121 = VECTOR ( 'NONE', #16104, 1000.000000000000000 ) ;
#22122 = DIRECTION ( 'NONE',  ( -1.213490492418603984E-15, -4.861311874477930828E-15, -1.000000000000000000 ) ) ;
#22123 = DIRECTION ( 'NONE',  ( 0.5249589903860194529, -0.8511275218278935295, 5.444325428271645316E-17 ) ) ;
#22124 = FACE_OUTER_BOUND ( 'NONE', #11696, .T. ) ;
#22125 = EDGE_CURVE ( 'NONE', #11752, #8111, #891, .T. ) ;
#22126 = CARTESIAN_POINT ( 'NONE',  ( 36.05760157943844035, 11.72988078058867245, 10.50000000000019185 ) ) ;
#22127 = CC_DESIGN_DATE_AND_TIME_ASSIGNMENT ( #2650, #4545, ( #22886 ) ) ;
#22128 = FACE_OUTER_BOUND ( 'NONE', #11959, .T. ) ;
#22129 = COORDINATED_UNIVERSAL_TIME_OFFSET ( 0, 0, .AHEAD. ) ;
#22130 = AXIS2_PLACEMENT_3D ( 'NONE', #4708, #6845, #17302 ) ;
#22131 = CC_DESIGN_DATE_AND_TIME_ASSIGNMENT ( #22229, #22696, ( #22038 ) ) ;
#22132 = DIRECTION ( 'NONE',  ( -2.982858504577314686E-17, 2.441916418604790135E-15, 1.000000000000000000 ) ) ;
#22133 = CARTESIAN_POINT ( 'NONE',  ( 2.500000000000000000, -17.30000000000000071, -2.500000000000000000 ) ) ;
#22134 = ADVANCED_FACE ( 'NONE', ( #13956 ), #4049, .F. ) ;
#22135 = EDGE_CURVE ( 'NONE', #10848, #23125, #15500, .T. ) ;
#22136 = CARTESIAN_POINT ( 'NONE',  ( -11.34268231757140022, -0.05939068843019929683, -2.500000000000090150 ) ) ;
#22137 = DIRECTION ( 'NONE',  ( -0.2306359803922031770, -0.9730401042858034533, 0.000000000000000000 ) ) ;
#22139 = EDGE_CURVE ( 'NONE', #19161, #16449, #22730, .T. ) ;
#22138 = LINE ( 'NONE', #10840, #11548 ) ;
#22140 = CARTESIAN_POINT ( 'NONE',  ( -26.99999999999959854, -33.09999999999999432, -22.00000000000000000 ) ) ;
#22141 = ORIENTED_EDGE ( 'NONE', *, *, #14365, .F. ) ;
#22142 = ORIENTED_EDGE ( 'NONE', *, *, #2595, .F. ) ;
#22143 = DIRECTION ( 'NONE',  ( -1.000000000000000000, 0.000000000000000000, 0.000000000000000000 ) ) ;
#22144 = CARTESIAN_POINT ( 'NONE',  ( 34.74128820227589642, 24.82052816820949914, -11.50000000000049916 ) ) ;
#22145 = ORIENTED_EDGE ( 'NONE', *, *, #3883, .F. ) ;
#22146 = DIRECTION ( 'NONE',  ( 0.9730401042858024541, -0.2306359803922080898, -5.959266323858942451E-17 ) ) ;
#22147 = AXIS2_PLACEMENT_3D ( 'NONE', #16964, #6161, #686 ) ;
#22148 = VERTEX_POINT ( 'NONE', #11731 ) ;
#22149 = DIRECTION ( 'NONE',  ( 0.000000000000000000, 0.000000000000000000, -1.000000000000000000 ) ) ;
#22150 = DATE_AND_TIME ( #3990, #3531 ) ;
#22151 = CARTESIAN_POINT ( 'NONE',  ( 37.57874659166015618, 10.36844021841513985, -8.940971698096582543 ) ) ;
#22152 = ADVANCED_FACE ( 'NONE', ( #9820 ), #20355, .F. ) ;
#22153 = CONTEXT_DEPENDENT_SHAPE_REPRESENTATION ( #12638, #12901 ) ;
#22154 =( NAMED_UNIT ( * ) PLANE_ANGLE_UNIT ( ) SI_UNIT ( $, .RADIAN. ) );
#22155 = DIRECTION ( 'NONE',  ( 0.9730401042858024541, -0.2306359803922080898, -5.959266323858942451E-17 ) ) ;
#22156 = ORIENTED_EDGE ( 'NONE', *, *, #8689, .F. ) ;
#22157 = CARTESIAN_POINT ( 'NONE',  ( 39.37089837072289811, 22.23982225285510239, 10.49999999999999822 ) ) ;
#22158 = ORIENTED_EDGE ( 'NONE', *, *, #7108, .T. ) ;
#22159 = DIRECTION ( 'NONE',  ( -2.979205983926755381E-09, 0.4472135954999659213, 0.8944271909999118586 ) ) ;
#22160 = EDGE_CURVE ( 'NONE', #3328, #1999, #23373, .T. ) ;
#22161 = EDGE_CURVE ( 'NONE', #21863, #11837, #1238, .T. ) ;
#22162 = CARTESIAN_POINT ( 'NONE',  ( 30.72899802076640086, 10.92798958341530025, -1.881607274541729715E-15 ) ) ;
#22163 = VERTEX_POINT ( 'NONE', #6473 ) ;
#22164 = PLANE ( 'NONE',  #16560 ) ;
#22165 = DIRECTION ( 'NONE',  ( -2.982858504577319616E-17, 2.441916418604790135E-15, 1.000000000000000000 ) ) ;
#22166 = CARTESIAN_POINT ( 'NONE',  ( -0.9605240398339689456, 18.43923599187829865, -8.566766326431390468E-17 ) ) ;
#22167 = ORIENTED_EDGE ( 'NONE', *, *, #16413, .F. ) ;
#22168 = COORDINATED_UNIVERSAL_TIME_OFFSET ( 0, 0, .AHEAD. ) ;
#22169 = DIRECTION ( 'NONE',  ( 0.000000000000000000, 0.000000000000000000, 1.000000000000000000 ) ) ;
#22170 = ORIENTED_EDGE ( 'NONE', *, *, #9701, .F. ) ;
#22171 = COORDINATED_UNIVERSAL_TIME_OFFSET ( 0, 0, .AHEAD. ) ;
#22172 = DIRECTION ( 'NONE',  ( 0.000000000000000000, 0.000000000000000000, -1.000000000000000000 ) ) ;
#22173 = ORIENTED_EDGE ( 'NONE', *, *, #22019, .F. ) ;
#22174 = ORIENTED_EDGE ( 'NONE', *, *, #13482, .F. ) ;
#22175 = CARTESIAN_POINT ( 'NONE',  ( -25.44852691694969948, 25.46424985927700035, 3.749999999999940048 ) ) ;
#22176 = DATE_TIME_ROLE ( 'classification_date' ) ;
#22177 = EDGE_CURVE ( 'NONE', #4383, #17959, #23027, .T. ) ;
#22178 = CIRCLE ( 'NONE', #18028, 2.500000000000000444 ) ;
#22179 = DATE_TIME_ROLE ( 'classification_date' ) ;
#22180 = DIRECTION ( 'NONE',  ( -6.123237831918409167E-17, 1.613784273878194890E-30, 1.000000000000000000 ) ) ;
#22181 =( NAMED_UNIT ( * ) SI_UNIT ( $, .STERADIAN. ) SOLID_ANGLE_UNIT ( ) );
#22182 = CARTESIAN_POINT ( 'NONE',  ( -31.64676348097539815, 7.334526001134540785, 5.000000000000000000 ) ) ;
#22183 = EDGE_CURVE ( 'NONE', #23121, #12383, #15203, .T. ) ;
#22184 = CALENDAR_DATE ( 2026, 31, 10 ) ;
#22185 = PRODUCT_DEFINITION_SHAPE ( 'NONE', 'NONE',  #23491 ) ;
#22186 = EDGE_CURVE ( 'NONE', #22407, #10583, #19191, .T. ) ;
#22187 = EDGE_LOOP ( 'NONE', ( #22111, #2966, #6650, #21491 ) ) ;
#22188 = APPLICATION_CONTEXT ( 'configuration controlled 3d designs of mechanical parts and assemblies' ) ;
#22189 = FACE_OUTER_BOUND ( 'NONE', #1165, .T. ) ;
#22190 = ORIENTED_EDGE ( 'NONE', *, *, #1254, .F. ) ;
#22191 = DIRECTION ( 'NONE',  ( 0.2306359803922031215, 0.9730401042858034533, -4.741332172907939802E-18 ) ) ;
#22192 =( GEOMETRIC_REPRESENTATION_CONTEXT ( 3 ) GLOBAL_UNCERTAINTY_ASSIGNED_CONTEXT ( ( #14183 ) ) GLOBAL_UNIT_ASSIGNED_CONTEXT ( ( #12086, #2807, #17653 ) ) REPRESENTATION_CONTEXT ( 'NONE', 'WORKASPACE' ) );
#22193 = DIRECTION ( 'NONE',  ( -1.000000000000000000, 1.982541115402065307E-15, 0.000000000000000000 ) ) ;
#22194 = SHAPE_REPRESENTATION ( '1602p_c_43', ( #12739 ), #5684 ) ;
#22195 = DIRECTION ( 'NONE',  ( 1.000000000000000000, -1.187319687680510101E-16, 0.000000000000000000 ) ) ;
#22196 = ORIENTED_EDGE ( 'NONE', *, *, #21803, .T. ) ;
#22197 = VERTEX_POINT ( 'NONE', #4810 ) ;
#22198 = CARTESIAN_POINT ( 'NONE',  ( 39.27359436029429673, 22.26288585089429972, 17.25000000000000000 ) ) ;
#22199 = ORIENTED_EDGE ( 'NONE', *, *, #17354, .F. ) ;
#22200 = PERSON_AND_ORGANIZATION ( #11966, #8758 ) ;
#22201 = ORIENTED_EDGE ( 'NONE', *, *, #22885, .F. ) ;
#22202 = ORIENTED_EDGE ( 'NONE', *, *, #3188, .T. ) ;
#22203 = CARTESIAN_POINT ( 'NONE',  ( 117.1933702072879981, -12.34113894325849969, -18.89999999999999858 ) ) ;
#22204 = LINE ( 'NONE', #6638, #4851 ) ;
#22205 = PERSON_AND_ORGANIZATION ( #11966, #8758 ) ;
#22206 = CARTESIAN_POINT ( 'NONE',  ( -29.94163891957289891, 6.343422587376370103, 5.000000000000000000 ) ) ;
#22207 = CARTESIAN_POINT ( 'NONE',  ( -17.50000000000000000, -19.99999998334472195, 8.000000000004533263 ) ) ;
#22208 = CC_DESIGN_DATE_AND_TIME_ASSIGNMENT ( #11125, #5986, ( #7139 ) ) ;
#22209 = VERTEX_POINT ( 'NONE', #22512 ) ;
#22210 = AXIS2_PLACEMENT_3D ( 'NONE', #9025, #11186, #9262 ) ;
#22211 = DIRECTION ( 'NONE',  ( 8.274327508162393116E-31, 2.054129435991050111E-15, 1.000000000000000000 ) ) ;
#22212 = PERSON_AND_ORGANIZATION_ROLE ( 'creator' ) ;
#22213 = VERTEX_POINT ( 'NONE', #18849 ) ;
#22214 = DIRECTION ( 'NONE',  ( 1.328968407691592047E-16, -2.538119502737155889E-14, -1.000000000000000000 ) ) ;
#22215 = LINE ( 'NONE', #362, #4815 ) ;
#22216 = ORIENTED_EDGE ( 'NONE', *, *, #10422, .F. ) ;
#22217 = CARTESIAN_POINT ( 'NONE',  ( 35.59419854219520118, 9.774809681453550780, 26.88000000000000256 ) ) ;
#22218 = DIRECTION ( 'NONE',  ( -1.000000000000000000, 0.000000000000000000, 0.000000000000000000 ) ) ;
#22219 = ORIENTED_EDGE ( 'NONE', *, *, #8800, .F. ) ;
#22220 = FACE_OUTER_BOUND ( 'NONE', #8878, .T. ) ;
#22221 = APPLICATION_PROTOCOL_DEFINITION ( 'international standard', 'config_control_design', 1994, #23228 ) ;
#22222 = ADVANCED_FACE ( 'NONE', ( #759 ), #6250, .T. ) ;
#22223 = VECTOR ( 'NONE', #16511, 1000.000000000000114 ) ;
#22224 = VERTEX_POINT ( 'NONE', #18108 ) ;
#22225 = ORIENTED_EDGE ( 'NONE', *, *, #13760, .T. ) ;
#22226 = DIRECTION ( 'NONE',  ( -1.751019220569994795E-16, -2.300154215587015208E-15, -1.000000000000000000 ) ) ;
#22227 = AXIS2_PLACEMENT_3D ( 'NONE', #19521, #2898, #4912 ) ;
#22228 = EDGE_LOOP ( 'NONE', ( #7417, #11989, #15370, #20862, #20458, #10141, #22632, #4029, #10842 ) ) ;
#22229 = DATE_AND_TIME ( #13345, #8028 ) ;
#22230 = DIRECTION ( 'NONE',  ( 0.9730401042858035643, -0.2306359803922028717, -5.432877459303547053E-17 ) ) ;
#22231 = CARTESIAN_POINT ( 'NONE',  ( -14.00000000144930112, -4.350228928435750042, -7.999999999996869171 ) ) ;
#22232 = PERSON_AND_ORGANIZATION_ROLE ( 'classification_officer' ) ;
#22233 = CYLINDRICAL_SURFACE ( 'NONE', #267, 3.750000000000000000 ) ;
#22234 = EDGE_CURVE ( 'NONE', #3328, #14157, #8969, .T. ) ;
#22235 = DIRECTION ( 'NONE',  ( 0.000000000000000000, 0.000000000000000000, -1.000000000000000000 ) ) ;
#22236 = LINE ( 'NONE', #22006, #2947 ) ;
#22237 = CALENDAR_DATE ( 2026, 31, 10 ) ;
#22238 = VECTOR ( 'NONE', #22392, 1000.000000000000227 ) ;
#22239 = AXIS2_PLACEMENT_3D ( 'NONE', #22656, #13527, #4499 ) ;
#22240 = AXIS2_PLACEMENT_3D ( 'NONE', #10402, #21172, #6452 ) ;
#22241 = CARTESIAN_POINT ( 'NONE',  ( 1.213484035536889882, 25.73383521926719908, -2.500000000000000000 ) ) ;
#22242 = DIRECTION ( 'NONE',  ( -3.210834492180725196E-17, 2.441916418604790135E-15, 1.000000000000000000 ) ) ;
#22243 = CARTESIAN_POINT ( 'NONE',  ( -20.00000000397270128, 22.95208919256889857, -4.999999999995559996 ) ) ;
#22244 = DIRECTION ( 'NONE',  ( -0.7071067811865475727, 1.387778780781445281E-15, 0.7071067811865475727 ) ) ;
#22245 = CYLINDRICAL_SURFACE ( 'NONE', #19475, 5.000000000000000888 ) ;
#22246 = DIRECTION ( 'NONE',  ( -0.9999862922474492821, -0.005235963827108258348, 0.000000000000000000 ) ) ;
#22247 = VERTEX_POINT ( 'NONE', #7080 ) ;
#22248 = ADVANCED_FACE ( 'NONE', ( #8861 ), #16202, .F. ) ;
#22249 = ORIENTED_EDGE ( 'NONE', *, *, #1355, .F. ) ;
#22250 = CARTESIAN_POINT ( 'NONE',  ( -19.52710366811739817, 1.147603427694330103, 5.000000000000000000 ) ) ;
#22251 = CARTESIAN_POINT ( 'NONE',  ( 35.59419854219520118, 9.774809681453550780, 26.88000000000000256 ) ) ;
#22252 = VECTOR ( 'NONE', #13218, 999.9999999999998863 ) ;
#22253 = VERTEX_POINT ( 'NONE', #1822 ) ;
#22254 = CC_DESIGN_PERSON_AND_ORGANIZATION_ASSIGNMENT ( #178, #3874, ( #1558 ) ) ;
#22255 = CARTESIAN_POINT ( 'NONE',  ( -16.50000000202710027, 1.899127378699190016, -6.749999999996310507 ) ) ;
#22256 = ORIENTED_EDGE ( 'NONE', *, *, #3455, .F. ) ;
#22257 = AXIS2_PLACEMENT_3D ( 'NONE', #13234, #20467, #5624 ) ;
#22258 = CARTESIAN_POINT ( 'NONE',  ( -20.00000000000000000, -20.00000000000000000, 8.000000000004559908 ) ) ;
#22259 = AXIS2_PLACEMENT_3D ( 'NONE', #3947, #18329, #20681 ) ;
#22260 = APPLICATION_PROTOCOL_DEFINITION ( 'international standard', 'config_control_design', 1994, #8221 ) ;
#22261 = CARTESIAN_POINT ( 'NONE',  ( 37.09915056617500539, 8.351545750134603097, -8.940674882554525027 ) ) ;
#22262 = ADVANCED_FACE ( 'NONE', ( #19536 ), #8245, .T. ) ;
#22263 = EDGE_CURVE ( 'NONE', #20801, #17589, #16962, .T. ) ;
#22264 = DATE_AND_TIME ( #15030, #17898 ) ;
#22265 = AXIS2_PLACEMENT_3D ( 'NONE', #5621, #9432, #7644 ) ;
#22266 =( LENGTH_UNIT ( ) NAMED_UNIT ( * ) SI_UNIT ( .MILLI., .METRE. ) );
#22267 = DIRECTION ( 'NONE',  ( -3.099353312215988811E-62, 0.000000000000000000, 1.000000000000000000 ) ) ;
#22268 = EDGE_LOOP ( 'NONE', ( #17288, #17810, #12215, #17795, #15458 ) ) ;
#22269 = CIRCLE ( 'NONE', #12075, 5.000000000000001776 ) ;
#22270 = LINE ( 'NONE', #20629, #19866 ) ;
#22271 = VERTEX_POINT ( 'NONE', #14299 ) ;
#22272 = CARTESIAN_POINT ( 'NONE',  ( -28.95596696049959817, -6.651703575491109355, -4.767474059747899950 ) ) ;
#22273 = VECTOR ( 'NONE', #20501, 1000.000000000000000 ) ;
#22274 = AXIS2_PLACEMENT_3D ( 'NONE', #15357, #2535, #974 ) ;
#22275 = CARTESIAN_POINT ( 'NONE',  ( -59.82876553991570034, -8.313375209878421046, -5.528360538656856695E-15 ) ) ;
#22276 = AXIS2_PLACEMENT_3D ( 'NONE', #16791, #5874, #14773 ) ;
#22277 = VERTEX_POINT ( 'NONE', #3496 ) ;
#22278 = FACE_OUTER_BOUND ( 'NONE', #18686, .T. ) ;
#22279 = DIRECTION ( 'NONE',  ( -0.4999931461237239749, -0.002617981913554110092, 0.8660254037844389297 ) ) ;
#22280 = VERTEX_POINT ( 'NONE', #3616 ) ;
#22281 = EDGE_CURVE ( 'NONE', #989, #3393, #8566, .T. ) ;
#22282 = PERSON_AND_ORGANIZATION_ROLE ( 'classification_officer' ) ;
#22283 = CARTESIAN_POINT ( 'NONE',  ( 52.26033179423370001, -7.535689554643993482, -10.50000000000039968 ) ) ;
#22284 = VECTOR ( 'NONE', #6866, 1000.000000000000000 ) ;
#22285 = ORIENTED_EDGE ( 'NONE', *, *, #5923, .F. ) ;
#22287 = CALENDAR_DATE ( 2026, 31, 10 ) ;
#22286 = PRODUCT_RELATED_PRODUCT_CATEGORY ( 'detail', '', ( #10100 ) ) ;
#22288 = DIRECTION ( 'NONE',  ( -0.2306359803922101437, -0.9730401042858018990, 4.373252460445732608E-15 ) ) ;
#22289 = EDGE_LOOP ( 'NONE', ( #20367, #21602, #18519, #5548 ) ) ;
#22290 = ORIENTED_EDGE ( 'NONE', *, *, #3720, .T. ) ;
#22291 = PRODUCT_DEFINITION ( 'UNKNOWN', '', #7614, #16321 ) ;
#22292 = CARTESIAN_POINT ( 'NONE',  ( -19.49999999982379961, -0.1021026942259709996, 2.500000000000090150 ) ) ;
#22293 = CALENDAR_DATE ( 2026, 31, 10 ) ;
#22294 = EDGE_CURVE ( 'NONE', #5571, #23086, #16201, .T. ) ;
#22295 = EDGE_CURVE ( 'NONE', #10657, #17206, #15965, .T. ) ;
#22296 = EDGE_CURVE ( 'NONE', #2989, #8934, #9779, .T. ) ;
#22297 = APPROVAL_DATE_TIME ( #20647, #15157 ) ;
#22298 = AXIS2_PLACEMENT_3D ( 'NONE', #23299, #12512, #10973 ) ;
#22299 = DIRECTION ( 'NONE',  ( 0.2306359803922022056, 0.9730401042858037863, -4.163336342344340971E-15 ) ) ;
#22300 = LINE ( 'NONE', #6040, #3157 ) ;
#22301 = EDGE_LOOP ( 'NONE', ( #17004, #21665, #3607, #11770 ) ) ;
#22302 = APPROVAL_DATE_TIME ( #18293, #659 ) ;
#22303 = VERTEX_POINT ( 'NONE', #14415 ) ;
#22304 = CARTESIAN_POINT ( 'NONE',  ( -16.50000000000000000, -20.00000000000000000, -2.500000000000000000 ) ) ;
#22305 = ORIENTED_EDGE ( 'NONE', *, *, #21771, .T. ) ;
#22306 = EDGE_CURVE ( 'NONE', #142, #21288, #7187, .T. ) ;
#22307 = DIRECTION ( 'NONE',  ( 0.9730401042858024541, -0.2306359803922080898, -5.959266323858942451E-17 ) ) ;
#22309 = VECTOR ( 'NONE', #14932, 1000.000000000000000 ) ;
#22308 = CARTESIAN_POINT ( 'NONE',  ( -19.63010143622448211, 27.93838792505352941, -5.499999999995570654 ) ) ;
#22310 = DIRECTION ( 'NONE',  ( -1.000000000000000000, 0.000000000000000000, -3.099353312215991402E-62 ) ) ;
#22311 = ORIENTED_EDGE ( 'NONE', *, *, #18591, .F. ) ;
#22312 = ORIENTED_EDGE ( 'NONE', *, *, #13991, .F. ) ;
#22313 = DIRECTION ( 'NONE',  ( 0.000000000000000000, 0.000000000000000000, -1.000000000000000000 ) ) ;
#22314 = ORIENTED_EDGE ( 'NONE', *, *, #7826, .F. ) ;
#22315 = PERSON_AND_ORGANIZATION_ROLE ( 'design_supplier' ) ;
#22316 = ADVANCED_FACE ( 'NONE', ( #18001 ), #16090, .T. ) ;
#22317 = ORIENTED_EDGE ( 'NONE', *, *, #22323, .T. ) ;
#22318 = EDGE_LOOP ( 'NONE', ( #16824, #6012, #15200, #4105 ) ) ;
#22319 = CARTESIAN_POINT ( 'NONE',  ( 36.78282996199610722, 11.03463321983559986, -27.69000000000049866 ) ) ;
#22320 = APPROVAL_DATE_TIME ( #823, #13443 ) ;
#22321 = EDGE_CURVE ( 'NONE', #12306, #9811, #21650, .T. ) ;
#22322 = DIRECTION ( 'NONE',  ( -0.9730401042858022320, 0.2306359803922080343, -2.396759184561635323E-31 ) ) ;
#22323 = EDGE_CURVE ( 'NONE', #20452, #23068, #10158, .T. ) ;
#22324 = CARTESIAN_POINT ( 'NONE',  ( -58.40964484538829993, -25.30627767975780174, 2.500000000000000000 ) ) ;
#22325 =( NAMED_UNIT ( * ) SI_UNIT ( $, .STERADIAN. ) SOLID_ANGLE_UNIT ( ) );
#22326 = CARTESIAN_POINT ( 'NONE',  ( 36.84099409957970295, 22.83947580187469839, -13.00000000000049916 ) ) ;
#22327 = APPROVAL_ROLE ( '' ) ;
#22328 =( BOUNDED_CURVE ( )  B_SPLINE_CURVE ( 2, ( #7892, #15011, #13239 ),
 .UNSPECIFIED., .F., .F. ) 
 B_SPLINE_CURVE_WITH_KNOTS ( ( 3, 3 ),
 ( 0.000000000000000000, 0.1752654207116860208 ),
 .UNSPECIFIED. ) 
 CURVE ( )  GEOMETRIC_REPRESENTATION_ITEM ( )  RATIONAL_B_SPLINE_CURVE ( ( 1.000000000000000000, 1.154700538379239916, 1.000000000000000000 ) ) 
 REPRESENTATION_ITEM ( '' )  );
#22329 = VERTEX_POINT ( 'NONE', #12321 ) ;
#22330 = CARTESIAN_POINT ( 'NONE',  ( -58.40964484538829993, -25.30627767975780174, 2.500000000000000000 ) ) ;
#22331 = AXIS2_PLACEMENT_3D ( 'NONE', #4780, #6804, #1079 ) ;
#22332 = LINE ( 'NONE', #16879, #9374 ) ;
#22333 = ORIENTED_EDGE ( 'NONE', *, *, #4516, .F. ) ;
#22334 = DIRECTION ( 'NONE',  ( 0.000000000000000000, 0.000000000000000000, 1.000000000000000000 ) ) ;
#22335 = CARTESIAN_POINT ( 'NONE',  ( 30.97225804683764139, 10.87033058831654131, 26.87999999999999545 ) ) ;
#22336 = ORIENTED_EDGE ( 'NONE', *, *, #10263, .T. ) ;
#22337 = FACE_OUTER_BOUND ( 'NONE', #14695, .T. ) ;
#22338 = APPROVAL ( #7028, 'UNSPECIFIED' ) ;
#22339 = APPROVAL_ROLE ( '' ) ;
#22340 = ORIENTED_EDGE ( 'NONE', *, *, #16315, .T. ) ;
#22341 = ORIENTED_EDGE ( 'NONE', *, *, #14300, .F. ) ;
#22342 = FACE_OUTER_BOUND ( 'NONE', #12316, .T. ) ;
#22343 = DIRECTION ( 'NONE',  ( 0.9730401042858024541, -0.2306359803922080898, -5.959266323858942451E-17 ) ) ;
#22344 = ORIENTED_EDGE ( 'NONE', *, *, #20132, .F. ) ;
#22345 = PERSON_AND_ORGANIZATION ( #11966, #8758 ) ;
#22346 = CARTESIAN_POINT ( 'NONE',  ( 39.69419854219519550, 9.774809681453278998, -21.50000000000000000 ) ) ;
#22347 = CARTESIAN_POINT ( 'NONE',  ( 31.56827854690370927, -0.8510906712623030890, -14.00000000000040146 ) ) ;
#22348 = CC_DESIGN_SECURITY_CLASSIFICATION ( #9089, ( #23485 ) ) ;
#22349 = DATE_AND_TIME ( #621, #2415 ) ;
#22350 = CIRCLE ( 'NONE', #4157, 4.099999999999999645 ) ;
#22351 = PLANE ( 'NONE',  #13197 ) ;
#22352 = CIRCLE ( 'NONE', #12892, 2.750000000000001332 ) ;
#22353 = FACE_OUTER_BOUND ( 'NONE', #9861, .T. ) ;
#22354 = ADVANCED_FACE ( 'NONE', ( #1587 ), #14069, .F. ) ;
#22355 = DIRECTION ( 'NONE',  ( 1.000000000000000000, -8.896220237034308570E-17, 0.000000000000000000 ) ) ;
#22356 = PERSON_AND_ORGANIZATION ( #11966, #8758 ) ;
#22357 = CARTESIAN_POINT ( 'NONE',  ( 3.242007008979478005E-15, -33.09999999999999432, -25.00000000000000000 ) ) ;
#22358 = CARTESIAN_POINT ( 'NONE',  ( 31.01827548281339375, -2.500766059351008153, 15.00000000000011369 ) ) ;
#22359 = DIRECTION ( 'NONE',  ( 0.9730401042858036753, -0.2306359803922031493, -5.959266323858673745E-17 ) ) ;
#22360 = LOCAL_TIME ( 14, 11, 27.00000000000000000, #5570 ) ;
#22361 = DIRECTION ( 'NONE',  ( -0.2306359803922033991, -0.9730401042858034533, 0.000000000000000000 ) ) ;
#22362 = CIRCLE ( 'NONE', #1886, 4.250000000000000000 ) ;
#22363 = AXIS2_PLACEMENT_3D ( 'NONE', #14518, #10396, #8831 ) ;
#22364 = CARTESIAN_POINT ( 'NONE',  ( -20.00000000000170175, -20.00000000000000000, -6.749999999995469402 ) ) ;
#22365 = AXIS2_PLACEMENT_3D ( 'NONE', #8814, #16047, #224 ) ;
#22366 = DIRECTION ( 'NONE',  ( -0.9730401042858024541, 0.2306359803922080898, 5.959266323859212389E-17 ) ) ;
#22367 = ORIENTED_EDGE ( 'NONE', *, *, #23038, .T. ) ;
#22368 = ORIENTED_EDGE ( 'NONE', *, *, #16726, .T. ) ;
#22369 = CARTESIAN_POINT ( 'NONE',  ( 28.67817383939640052, -0.7594070262927701265, -11.00000000000039968 ) ) ;
#22370 = DIRECTION ( 'NONE',  ( -0.7070970883417637687, -0.003702385528197202434, 0.7071067811865479058 ) ) ;
#22371 = ORIENTED_EDGE ( 'NONE', *, *, #14014, .F. ) ;
#22372 = PERSON ( 'NAUO-PER39', 'UNSPECIFIED', 'UNSPECIFIED', ('UNSPECIFIED'), ('UNSPECIFIED'), ('UNSPECIFIED') ) ;
#22373 = VECTOR ( 'NONE', #22214, 1000.000000000000000 ) ;
#22374 = LINE ( 'NONE', #4351, #12635 ) ;
#22375 = ORIENTED_EDGE ( 'NONE', *, *, #14467, .T. ) ;
#22376 = CARTESIAN_POINT ( 'NONE',  ( 43.45766680872420551, 21.27115113520920175, -13.00000000000000000 ) ) ;
#22377 = AXIS2_PLACEMENT_3D ( 'NONE', #12738, #20079, #4051 ) ;
#22378 = PERSON_AND_ORGANIZATION ( #11966, #8758 ) ;
#22379 = DIRECTION ( 'NONE',  ( -1.000000000000000000, 0.000000000000000000, 0.000000000000000000 ) ) ;
#22380 = PRODUCT_DEFINITION_SHAPE ( 'NONE', 'NONE',  #23481 ) ;
#22381 = CC_DESIGN_APPROVAL ( #15337, ( #20495 ) ) ;
#22382 = CONTEXT_DEPENDENT_SHAPE_REPRESENTATION ( #6418, #370 ) ;
#22383 = DIRECTION ( 'NONE',  ( -3.099353312215989243E-62, 1.534091707905539548E-92, 1.000000000000000000 ) ) ;
#22384 = VERTEX_POINT ( 'NONE', #10529 ) ;
#22385 = EDGE_CURVE ( 'NONE', #10964, #990, #2562, .T. ) ;
#22386 = PLANE ( 'NONE',  #128 ) ;
#22387 = EDGE_LOOP ( 'NONE', ( #19461, #6055, #13258, #7101 ) ) ;
#22389 = AXIS2_PLACEMENT_3D ( 'NONE', #4765, #13907, #12265 ) ;
#22388 = CARTESIAN_POINT ( 'NONE',  ( -14.00000000397270128, 22.95208919312850071, 6.750000000004400036 ) ) ;
#22390 = CC_DESIGN_PERSON_AND_ORGANIZATION_ASSIGNMENT ( #8748, #10443, ( #1162 ) ) ;
#22391 = VERTEX_POINT ( 'NONE', #10644 ) ;
#22392 = DIRECTION ( 'NONE',  ( -0.2306359803922080343, -0.9730401042858022320, 1.412237191019910313E-17 ) ) ;
#22393 = CARTESIAN_POINT ( 'NONE',  ( -65.64475015647069256, -21.84411297095480009, -5.000000000000000000 ) ) ;
#22394 = ORIENTED_EDGE ( 'NONE', *, *, #10452, .T. ) ;
#22395 = ADVANCED_FACE ( 'NONE', ( #10773 ), #21535, .T. ) ;
#22396 = CLOSED_SHELL ( 'NONE', ( #1865, #8132, #20133, #15034, #11805, #15782, #10097, #11593, #4583, #707, #2048, #1112, #18431, #12972, #18567, #1996, #22853, #3967, #2900, #9935, #9247 ) ) ;
#22397 = ADVANCED_FACE ( 'NONE', ( #18707 ), #10548, .F. ) ;
#22398 = UNCERTAINTY_MEASURE_WITH_UNIT (LENGTH_MEASURE( 1.000000000000000082E-05 ), #19948, 'distance_accuracy_value', 'NONE');
#22399 = LOCAL_TIME ( 14, 11, 27.00000000000000000, #3896 ) ;
#22400 = DATE_TIME_ROLE ( 'classification_date' ) ;
#22401 = CARTESIAN_POINT ( 'NONE',  ( 112.6956120935907251, 3.369770385951718517, -2.066999999999968196 ) ) ;
#22402 = LOCAL_TIME ( 14, 11, 27.00000000000000000, #3971 ) ;
#22403 = VERTEX_POINT ( 'NONE', #12763 ) ;
#22404 = SHAPE_DEFINITION_REPRESENTATION ( #10453, #19303 ) ;
#22405 = CARTESIAN_POINT ( 'NONE',  ( -18.05391955182270181, 22.49081825942809942, -4.900728725074969882E-15 ) ) ;
#22406 = CIRCLE ( 'NONE', #14076, 4.999999999999997335 ) ;
#22407 = VERTEX_POINT ( 'NONE', #9685 ) ;
#22408 = VERTEX_POINT ( 'NONE', #7883 ) ;
#22409 = FACE_OUTER_BOUND ( 'NONE', #15130, .T. ) ;
#22410 = EDGE_CURVE ( 'NONE', #15703, #12824, #13935, .T. ) ;
#22411 = CC_DESIGN_SECURITY_CLASSIFICATION ( #1928, ( #23488 ) ) ;
#22412 = PERSON_AND_ORGANIZATION_ROLE ( 'creator' ) ;
#22413 = CALENDAR_DATE ( 2026, 31, 10 ) ;
#22414 = PLANE ( 'NONE',  #7035 ) ;
#22415 = ADVANCED_FACE ( 'NONE', ( #9556 ), #14689, .F. ) ;
#22416 = CC_DESIGN_APPROVAL ( #11587, ( #6637 ) ) ;
#22417 = CC_DESIGN_SECURITY_CLASSIFICATION ( #4599, ( #11077 ) ) ;
#22418 = DIRECTION ( 'NONE',  ( -3.210834492181180024E-17, 2.441916418604790135E-15, 1.000000000000000000 ) ) ;
#22419 = VECTOR ( 'NONE', #14608, 1000.000000000000114 ) ;
#22420 = EDGE_LOOP ( 'NONE', ( #10883, #8043, #222, #19348 ) ) ;
#22421 = CC_DESIGN_PERSON_AND_ORGANIZATION_ASSIGNMENT ( #5773, #2565, ( #10854 ) ) ;
#22422 = PERSON_AND_ORGANIZATION_ROLE ( 'classification_officer' ) ;
#22423 = CC_DESIGN_PERSON_AND_ORGANIZATION_ASSIGNMENT ( #18517, #22530, ( #19768 ) ) ;
#22424 = EDGE_LOOP ( 'NONE', ( #107, #18600, #18759, #17884 ) ) ;
#22425 = APPROVAL_PERSON_ORGANIZATION ( #17323, #23407, #12349 ) ;
#22426 = CARTESIAN_POINT ( 'NONE',  ( -4.514225866272930432, 4.676725866273569565, 2.500000000000000000 ) ) ;
#22427 = CARTESIAN_POINT ( 'NONE',  ( -23.49893655333878684, 22.87624079303554581, 3.749999999999900080 ) ) ;
#22428 = ORIENTED_EDGE ( 'NONE', *, *, #15449, .F. ) ;
#22429 = EDGE_CURVE ( 'NONE', #1608, #1750, #7497, .T. ) ;
#22430 = ADVANCED_FACE ( 'NONE', ( #12875 ), #2064, .F. ) ;
#22431 = CARTESIAN_POINT ( 'NONE',  ( -21.66397194015859640, 11.15562530387989959, -2.500000000000000000 ) ) ;
#22432 = APPROVAL ( #11652, 'UNSPECIFIED' ) ;
#22433 = DIRECTION ( 'NONE',  ( 0.000000000000000000, -1.000000000000000000, 9.355573283744330345E-16 ) ) ;
#22434 = DIRECTION ( 'NONE',  ( -2.270069654138865127E-15, -1.000000000000000000, 4.574083617919690056E-30 ) ) ;
#22435 = ORIENTED_EDGE ( 'NONE', *, *, #14769, .T. ) ;
#22436 = ORIENTED_EDGE ( 'NONE', *, *, #236, .F. ) ;
#22437 = CYLINDRICAL_SURFACE ( 'NONE', #8351, 3.499999999999999112 ) ;
#22438 = VERTEX_POINT ( 'NONE', #1937 ) ;
#22439 = APPROVAL_ROLE ( '' ) ;
#22440 = CC_DESIGN_SECURITY_CLASSIFICATION ( #5001, ( #7661 ) ) ;
#22441 = ORIENTED_EDGE ( 'NONE', *, *, #3410, .T. ) ;
#22442 = ORIENTED_EDGE ( 'NONE', *, *, #3571, .T. ) ;
#22443 = CARTESIAN_POINT ( 'NONE',  ( 117.1933702072879981, -12.34113894325840022, 18.89999999999999858 ) ) ;
#22444 = PERSON_AND_ORGANIZATION_ROLE ( 'classification_officer' ) ;
#22445 = VECTOR ( 'NONE', #18203, 999.9999999999998863 ) ;
#22446 = DIRECTION ( 'NONE',  ( -0.2306359803922027607, -0.9730401042858035643, 0.000000000000000000 ) ) ;
#22447 = DIRECTION ( 'NONE',  ( 0.2306359803922017615, 0.9730401042858037863, -3.356987858687580135E-15 ) ) ;
#22448 = CC_DESIGN_SECURITY_CLASSIFICATION ( #19794, ( #23502 ) ) ;
#22449 = EDGE_CURVE ( 'NONE', #21101, #5291, #19243, .T. ) ;
#22450 = CIRCLE ( 'NONE', #1972, 6.500000000000000888 ) ;
#22451 =( NAMED_UNIT ( * ) PLANE_ANGLE_UNIT ( ) SI_UNIT ( $, .RADIAN. ) );
#22452 = DIRECTION ( 'NONE',  ( 6.123237831918399306E-17, -1.569224110909209817E-30, -1.000000000000000000 ) ) ;
#22453 = DATE_AND_TIME ( #22800, #17499 ) ;
#22454 = APPROVAL_PERSON_ORGANIZATION ( #17704, #12161, #1520 ) ;
#22455 = EDGE_LOOP ( 'NONE', ( #19040, #6532, #14409, #14412 ) ) ;
#22456 = CYLINDRICAL_SURFACE ( 'NONE', #1897, 4.099999999999999645 ) ;
#22457 = VECTOR ( 'NONE', #16637, 1000.000000000000000 ) ;
#22458 = LINE ( 'NONE', #7622, #13925 ) ;
#22459 = ORIENTED_EDGE ( 'NONE', *, *, #19963, .F. ) ;
#22460 = ADVANCED_FACE ( 'NONE', ( #16900 ), #11237, .F. ) ;
#22461 = CIRCLE ( 'NONE', #2003, 2.499999999999999112 ) ;
#22462 = EDGE_CURVE ( 'NONE', #7573, #3681, #7646, .T. ) ;
#22463 = DIRECTION ( 'NONE',  ( 3.210834492194360164E-17, -2.441916418604790135E-15, -1.000000000000000000 ) ) ;
#22464 = CARTESIAN_POINT ( 'NONE',  ( 61.93563330948219203, 19.01565939351215206, 13.00000000000000000 ) ) ;
#22465 = VERTEX_POINT ( 'NONE', #19999 ) ;
#22466 = CARTESIAN_POINT ( 'NONE',  ( 117.0319250210129951, -13.02226701625849969, -18.89999999999999858 ) ) ;
#22467 = APPLICATION_CONTEXT ( 'configuration controlled 3d designs of mechanical parts and assemblies' ) ;
#22468 = COORDINATED_UNIVERSAL_TIME_OFFSET ( 0, 0, .AHEAD. ) ;
#22469 = ORIENTED_EDGE ( 'NONE', *, *, #12962, .F. ) ;
#22470 = ORIENTED_EDGE ( 'NONE', *, *, #12586, .T. ) ;
#22471 = DIRECTION ( 'NONE',  ( 1.000000000000000000, 9.250482324585361611E-11, -2.269018306577663175E-13 ) ) ;
#22472 = CARTESIAN_POINT ( 'NONE',  ( 34.24699604337060066, 12.59578995394270073, 2.499999999999970246 ) ) ;
#22473 = AXIS2_PLACEMENT_3D ( 'NONE', #14595, #12592, #19940 ) ;
#22474 = CARTESIAN_POINT ( 'NONE',  ( -26.68881687192900287, -6.639832696913689603, 2.500292893218909906 ) ) ;
#22475 = COORDINATED_UNIVERSAL_TIME_OFFSET ( 0, 0, .AHEAD. ) ;
#22476 = CARTESIAN_POINT ( 'NONE',  ( 114.6071564266699880, -22.31351932764730250, 13.00000000000000000 ) ) ;
#22477 = CC_DESIGN_APPROVAL ( #19836, ( #10711 ) ) ;
#22478 = DIRECTION ( 'NONE',  ( 0.9730401042858033422, -0.2306359803922031215, 3.994774879569051239E-16 ) ) ;
#22479 = CALENDAR_DATE ( 2026, 31, 10 ) ;
#22480 = VECTOR ( 'NONE', #12466, 1000.000000000000114 ) ;
#22481 = FACE_OUTER_BOUND ( 'NONE', #14591, .T. ) ;
#22482 = CIRCLE ( 'NONE', #11136, 3.750000000000000000 ) ;
#22483 = ADVANCED_FACE ( 'NONE', ( #9435 ), #22233, .T. ) ;
#22484 = CIRCLE ( 'NONE', #2006, 2.750000000000001332 ) ;
#22485 =( BOUNDED_CURVE ( )  B_SPLINE_CURVE ( 2, ( #17744, #1450, #8713 ),
 .UNSPECIFIED., .F., .F. ) 
 B_SPLINE_CURVE_WITH_KNOTS ( ( 3, 3 ),
 ( 0.000000000000000000, 0.1752654207116860208 ),
 .UNSPECIFIED. ) 
 CURVE ( )  GEOMETRIC_REPRESENTATION_ITEM ( )  RATIONAL_B_SPLINE_CURVE ( ( 1.000000000000000000, 1.154700538379249908, 1.000000000000000000 ) ) 
 REPRESENTATION_ITEM ( '' )  );
#22486 = EDGE_CURVE ( 'NONE', #16965, #3768, #14655, .T. ) ;
#22487 = CARTESIAN_POINT ( 'NONE',  ( -64.07944010525035594, -25.33596492959100033, -5.000000000000000888 ) ) ;
#22488 = PERSON_AND_ORGANIZATION_ROLE ( 'classification_officer' ) ;
#22489 = ADVANCED_FACE ( 'NONE', ( #5979 ), #22647, .T. ) ;
#22490 = LINE ( 'NONE', #22241, #1283 ) ;
#22491 = AXIS2_PLACEMENT_3D ( 'NONE', #7649, #4200, #14889 ) ;
#22492 = CARTESIAN_POINT ( 'NONE',  ( 35.93893384793820189, -10.44995626450799975, -2.700000000000000178 ) ) ;
#22493 = AXIS2_PLACEMENT_3D ( 'NONE', #4267, #17325, #18648 ) ;
#22494 = ADVANCED_FACE ( 'NONE', ( #22124 ), #155, .T. ) ;
#22495 = CARTESIAN_POINT ( 'NONE',  ( -20.00000000000149925, -20.00000000000000000, -6.499999999995289990 ) ) ;
#22496 = CC_DESIGN_APPROVAL ( #2413, ( #5427 ) ) ;
#22497 = CARTESIAN_POINT ( 'NONE',  ( 37.46113131852559519, -4.027891576222994985, 13.00000000000000000 ) ) ;
#22498 = AXIS2_PLACEMENT_3D ( 'NONE', #21493, #19373, #12147 ) ;
#22499 = CARTESIAN_POINT ( 'NONE',  ( -19.44579266323601985, -2.601514938066530114, -2.499999999999993783 ) ) ;
#22500 = CIRCLE ( 'NONE', #20236, 15.25000000000000355 ) ;
#22501 = ORIENTED_EDGE ( 'NONE', *, *, #13891, .T. ) ;
#22502 = CIRCLE ( 'NONE', #17956, 12.49999999999999467 ) ;
#22503 = VERTEX_POINT ( 'NONE', #20350 ) ;
#22504 = DIRECTION ( 'NONE',  ( 1.000000000000000000, 2.874764335373299684E-17, 8.758115402030109610E-48 ) ) ;
#22505 = CARTESIAN_POINT ( 'NONE',  ( -16.50000000000000000, -20.00000000000000000, 0.000000000000000000 ) ) ;
#22506 = ORIENTED_EDGE ( 'NONE', *, *, #12336, .F. ) ;
#22507 = DIRECTION ( 'NONE',  ( 0.005225493764075828107, -0.9999863470142589250, 2.602085213965210642E-15 ) ) ;
#22508 = VERTEX_POINT ( 'NONE', #5868 ) ;
#22509 = CARTESIAN_POINT ( 'NONE',  ( -20.00000000000000000, -25.00000000000000000, 5.000000000004570566 ) ) ;
#22510 = AXIS2_PLACEMENT_3D ( 'NONE', #5942, #18666, #15086 ) ;
#22511 = CALENDAR_DATE ( 2026, 31, 10 ) ;
#22512 = CARTESIAN_POINT ( 'NONE',  ( -60.55739833509119308, 13.68311121755568394, -5.807568938802639321E-15 ) ) ;
#22513 = AXIS2_PLACEMENT_3D ( 'NONE', #15275, #2334, #19088 ) ;
#22514 = COORDINATED_UNIVERSAL_TIME_OFFSET ( 0, 0, .AHEAD. ) ;
#22515 = DIRECTION ( 'NONE',  ( 0.000000000000000000, 0.000000000000000000, 1.000000000000000000 ) ) ;
#22516 = AXIS2_PLACEMENT_3D ( 'NONE', #21017, #12010, #11554 ) ;
#22517 = DIRECTION ( 'NONE',  ( -0.2306359803922028995, -0.9730401042858034533, 4.741332172907957521E-18 ) ) ;
#22518 = APPROVAL ( #6449, 'UNSPECIFIED' ) ;
#22519 = CARTESIAN_POINT ( 'NONE',  ( 26.11627841292210306, -8.532812502301720059, -16.00000000000000000 ) ) ;
#22520 = ORIENTED_EDGE ( 'NONE', *, *, #8208, .F. ) ;
#22521 = DIRECTION ( 'NONE',  ( -0.9730401042858036753, 0.2306359803922028995, 5.958148513035547083E-17 ) ) ;
#22522 = FACE_OUTER_BOUND ( 'NONE', #8802, .T. ) ;
#22523 = ORIENTED_EDGE ( 'NONE', *, *, #6305, .T. ) ;
#22524 = FACE_OUTER_BOUND ( 'NONE', #4477, .T. ) ;
#22525 = CARTESIAN_POINT ( 'NONE',  ( -17.47493719149670000, 26.45208920939580111, 5.500000000004429346 ) ) ;
#22526 = DATE_AND_TIME ( #6142, #11868 ) ;
#22527 = CARTESIAN_POINT ( 'NONE',  ( -24.86147400983239919, -14.96352599016710094, -5.000000000000000000 ) ) ;
#22528 = AXIS2_PLACEMENT_3D ( 'NONE', #17691, #1163, #4856 ) ;
#22529 = VERTEX_POINT ( 'NONE', #13118 ) ;
#22530 = PERSON_AND_ORGANIZATION_ROLE ( 'design_supplier' ) ;
#22531 = CARTESIAN_POINT ( 'NONE',  ( 35.59419854219520118, 9.774809681453559662, 29.25000000000000000 ) ) ;
#22532 = EDGE_CURVE ( 'NONE', #15230, #13535, #8264, .T. ) ;
#22533 = ORIENTED_EDGE ( 'NONE', *, *, #20669, .F. ) ;
#22534 = VERTEX_POINT ( 'NONE', #3837 ) ;
#22535 = COORDINATED_UNIVERSAL_TIME_OFFSET ( 0, 0, .AHEAD. ) ;
#22536 = CALENDAR_DATE ( 2026, 31, 10 ) ;
#22537 = DIRECTION ( 'NONE',  ( -0.2306359803922094498, -0.9730401042858020100, 1.412237191019847142E-17 ) ) ;
#22538 = EDGE_CURVE ( 'NONE', #21501, #9873, #21133, .T. ) ;
#22539 = DIRECTION ( 'NONE',  ( 2.269747459788999852E-13, 2.220446049250325308E-15, 1.000000000000000000 ) ) ;
#22540 = ORIENTED_EDGE ( 'NONE', *, *, #21966, .F. ) ;
#22541 = SECURITY_CLASSIFICATION_LEVEL ( 'unclassified' ) ;
#22542 = ORIENTED_EDGE ( 'NONE', *, *, #22896, .F. ) ;
#22543 = FACE_OUTER_BOUND ( 'NONE', #19381, .T. ) ;
#22544 = VERTEX_POINT ( 'NONE', #19170 ) ;
#22545 = CYLINDRICAL_SURFACE ( 'NONE', #15471, 2.500000000000000444 ) ;
#22546 = CYLINDRICAL_SURFACE ( 'NONE', #12684, 2.067000000000000171 ) ;
#22547 = LINE ( 'NONE', #1043, #3146 ) ;
#22548 = ORIENTED_EDGE ( 'NONE', *, *, #11437, .T. ) ;
#22549 = EDGE_LOOP ( 'NONE', ( #1894, #20543 ) ) ;
#22550 = DIRECTION ( 'NONE',  ( -0.9730401042858035643, 0.2306359803922028717, 5.958148513035547083E-17 ) ) ;
#22551 = ORIENTED_EDGE ( 'NONE', *, *, #8477, .F. ) ;
#22552 = COORDINATED_UNIVERSAL_TIME_OFFSET ( 0, 0, .AHEAD. ) ;
#22553 = EDGE_CURVE ( 'NONE', #18764, #9785, #2890, .T. ) ;
#22554 = ORIENTED_EDGE ( 'NONE', *, *, #15631, .T. ) ;
#22555 = AXIS2_PLACEMENT_3D ( 'NONE', #4381, #15062, #22299 ) ;
#22556 = EDGE_LOOP ( 'NONE', ( #3791, #7757 ) ) ;
#22557 = CARTESIAN_POINT ( 'NONE',  ( 35.59419854219520118, 9.774809681453278998, -27.19000000000049866 ) ) ;
#22558 = PERSON_AND_ORGANIZATION_ROLE ( 'design_supplier' ) ;
#22559 = CC_DESIGN_PERSON_AND_ORGANIZATION_ASSIGNMENT ( #13348, #17017, ( #18743 ) ) ;
#22560 = APPROVAL ( #1325, 'UNSPECIFIED' ) ;
#22561 = CARTESIAN_POINT ( 'NONE',  ( 33.27705887009690144, -3.036156860537079893, 13.00000000000019895 ) ) ;
#22562 = ADVANCED_FACE ( 'NONE', ( #22481 ), #2998, .T. ) ;
#22563 = EDGE_CURVE ( 'NONE', #563, #18262, #19051, .T. ) ;
#22564 = LINE ( 'NONE', #18907, #21546 ) ;
#22565 = CALENDAR_DATE ( 2026, 31, 10 ) ;
#22566 = ORIENTED_EDGE ( 'NONE', *, *, #945, .T. ) ;
#22567 = DIRECTION ( 'NONE',  ( 0.9999862922474493931, 0.005235963827116132258, 3.478334803857182996E-33 ) ) ;
#22568 = PLANE ( 'NONE',  #20761 ) ;
#22569 = EDGE_LOOP ( 'NONE', ( #11063, #18577, #11488, #15928, #8902 ) ) ;
#22570 = CARTESIAN_POINT ( 'NONE',  ( -57.16110402867079898, 11.90787760832819941, 3.218044905330409686E-15 ) ) ;
#22571 = DIRECTION ( 'NONE',  ( -1.000000000000000000, 2.775557561562891351E-15, 0.000000000000000000 ) ) ;
#22572 = EDGE_LOOP ( 'NONE', ( #931, #3610 ) ) ;
#22573 = FACE_BOUND ( 'NONE', #17635, .T. ) ;
#22574 = DATE_AND_TIME ( #16887, #21251 ) ;
#22575 = ADVANCED_FACE ( 'NONE', ( #13576 ), #10270, .F. ) ;
#22576 = PRODUCT_DEFINITION_SHAPE ( 'NONE', 'NONE',  #23477 ) ;
#22577 = ORIENTED_EDGE ( 'NONE', *, *, #6230, .F. ) ;
#22578 = EDGE_LOOP ( 'NONE', ( #7016, #23280, #11251, #1752 ) ) ;
#22579 = CARTESIAN_POINT ( 'NONE',  ( 36.09092202081949807, 8.115512906978469942, 28.46999999999999886 ) ) ;
#22580 = FACE_OUTER_BOUND ( 'NONE', #17865, .T. ) ;
#22581 = ORIENTED_EDGE ( 'NONE', *, *, #8544, .T. ) ;
#22582 = PERSON_AND_ORGANIZATION ( #11966, #8758 ) ;
#22583 = CYLINDRICAL_SURFACE ( 'NONE', #20979, 2.066999999999999726 ) ;
#22584 = CC_DESIGN_PERSON_AND_ORGANIZATION_ASSIGNMENT ( #19483, #2968, ( #8452 ) ) ;
#22585 = CC_DESIGN_PERSON_AND_ORGANIZATION_ASSIGNMENT ( #13918, #14622, ( #14054 ) ) ;
#22586 = DIRECTION ( 'NONE',  ( 0.9730401042858035643, -0.2306359803922028717, -5.959266323858667582E-17 ) ) ;
#22587 = DIRECTION ( 'NONE',  ( -0.2306359803922080898, -0.9730401042858024541, 2.572202231434325988E-16 ) ) ;
#22588 = EDGE_CURVE ( 'NONE', #3674, #22084, #8131, .T. ) ;
#22589 = EDGE_CURVE ( 'NONE', #18063, #21559, #646, .T. ) ;
#22590 = VECTOR ( 'NONE', #17936, 999.9999999999998863 ) ;
#22591 = CARTESIAN_POINT ( 'NONE',  ( -20.00000000397459843, 22.95208919256889857, -8.249999999995548450 ) ) ;
#22592 = SECURITY_CLASSIFICATION_LEVEL ( 'unclassified' ) ;
#22593 = DIRECTION ( 'NONE',  ( -0.9999862922474491711, -0.005235963827128302210, 1.239088197126291310E-16 ) ) ;
#22594 = DIRECTION ( 'NONE',  ( -9.248937406224699144E-11, 1.000000000000000000, -2.220446028257580150E-15 ) ) ;
#22595 = DIRECTION ( 'NONE',  ( 1.000000000000000000, -1.187319687680499994E-16, 0.000000000000000000 ) ) ;
#22596 = DIRECTION ( 'NONE',  ( 0.005235963827117091560, -0.9999862922474493931, -2.636227439666999735E-16 ) ) ;
#22597 = CARTESIAN_POINT ( 'NONE',  ( -11.34268231757140022, -0.05939068843019999766, 2.500000000000090150 ) ) ;
#22598 = DIRECTION ( 'NONE',  ( 0.2306359803921919083, 0.9730401042858062288, 1.301042606982611127E-13 ) ) ;
#22599 = ORIENTED_EDGE ( 'NONE', *, *, #21315, .T. ) ;
#22600 = AXIS2_PLACEMENT_3D ( 'NONE', #23370, #1302, #15686 ) ;
#22601 = EDGE_CURVE ( 'NONE', #22900, #9333, #1029, .T. ) ;
#22602 = VERTEX_POINT ( 'NONE', #17138 ) ;
#22603 = PLANE ( 'NONE',  #10745 ) ;
#22604 = CARTESIAN_POINT ( 'NONE',  ( -16.30123784160759826, 29.88528286632680064, 2.500000000000000000 ) ) ;
#22605 = EDGE_LOOP ( 'NONE', ( #2061, #3899, #1372, #11181 ) ) ;
#22606 = LINE ( 'NONE', #18736, #3884 ) ;
#22607 = ORIENTED_EDGE ( 'NONE', *, *, #1857, .T. ) ;
#22608 = LINE ( 'NONE', #11842, #20476 ) ;
#22609 =( BOUNDED_CURVE ( )  B_SPLINE_CURVE ( 2, ( #2023, #109, #12722 ),
 .UNSPECIFIED., .F., .F. ) 
 B_SPLINE_CURVE_WITH_KNOTS ( ( 3, 3 ),
 ( 0.000000000000000000, 0.2928548593876180162 ),
 .UNSPECIFIED. ) 
 CURVE ( )  GEOMETRIC_REPRESENTATION_ITEM ( )  RATIONAL_B_SPLINE_CURVE ( ( 1.000000000000000000, 1.037954849302049842, 1.000000000000000000 ) ) 
 REPRESENTATION_ITEM ( '' )  );
#22610 = DATE_TIME_ROLE ( 'creation_date' ) ;
#22611 = LINE ( 'NONE', #9944, #1759 ) ;
#22612 = ADVANCED_FACE ( 'NONE', ( #13471 ), #13823, .T. ) ;
#22613 = AXIS2_PLACEMENT_3D ( 'NONE', #7051, #10738, #10969 ) ;
#22614 = ADVANCED_FACE ( 'NONE', ( #4547 ), #22351, .T. ) ;
#22615 = DATE_TIME_ROLE ( 'classification_date' ) ;
#22616 = AXIS2_PLACEMENT_3D ( 'NONE', #6591, #19060, #15601 ) ;
#22617 = AXIS2_PLACEMENT_3D ( 'NONE', #12970, #18448, #18803 ) ;
#22618 = DIRECTION ( 'NONE',  ( -0.7070970883417647679, -0.003702385528188428636, -0.7071067811865467956 ) ) ;
#22619 = CARTESIAN_POINT ( 'NONE',  ( 117.0319250210129951, -13.02226701625859917, 18.89999999999999858 ) ) ;
#22620 = DIRECTION ( 'NONE',  ( 0.000000000000000000, 0.000000000000000000, -1.000000000000000000 ) ) ;
#22621 = ORIENTED_EDGE ( 'NONE', *, *, #9589, .F. ) ;
#22622 = LINE ( 'NONE', #16689, #22273 ) ;
#22623 = CARTESIAN_POINT ( 'NONE',  ( 120.3930287342899987, 3.035456073538439714, -13.00000000000000000 ) ) ;
#22624 = ORIENTED_EDGE ( 'NONE', *, *, #2135, .F. ) ;
#22625 = CIRCLE ( 'NONE', #18483, 4.750000000000000000 ) ;
#22626 = CARTESIAN_POINT ( 'NONE',  ( -26.72214353971689960, -0.1399180949199879953, -2.500999999999910184 ) ) ;
#22627 = CARTESIAN_POINT ( 'NONE',  ( -22.50000000000000000, -20.00000000000000000, 5.000000000000000000 ) ) ;
#22628 = VECTOR ( 'NONE', #18741, 1000.000000000000000 ) ;
#22629 = DATE_AND_TIME ( #10200, #11098 ) ;
#22630 = CARTESIAN_POINT ( 'NONE',  ( 28.89837840081079889, -1.998294948772165736, 17.25000000000019895 ) ) ;
#22631 = AXIS2_PLACEMENT_3D ( 'NONE', #8359, #12177, #2896 ) ;
#22632 = ORIENTED_EDGE ( 'NONE', *, *, #13142, .F. ) ;
#22633 = ORIENTED_EDGE ( 'NONE', *, *, #7750, .F. ) ;
#22634 = CC_DESIGN_DATE_AND_TIME_ASSIGNMENT ( #22453, #2750, ( #2323 ) ) ;
#22635 = SHAPE_DEFINITION_REPRESENTATION ( #17820, #10375 ) ;
#22636 = DIRECTION ( 'NONE',  ( 0.9999863470142587030, 0.005225493764090578461, 1.706795877867719251E-17 ) ) ;
#22637 = EDGE_LOOP ( 'NONE', ( #17860, #11165 ) ) ;
#22638 = DIRECTION ( 'NONE',  ( 0.1997366180463766849, 0.8426774492125652660, -0.5000000000000004441 ) ) ;
#22639 = VECTOR ( 'NONE', #22123, 1000.000000000000000 ) ;
#22640 = APPLICATION_CONTEXT ( 'configuration controlled 3d designs of mechanical parts and assemblies' ) ;
#22641 = APPROVAL_DATE_TIME ( #20869, #10120 ) ;
#22642 = PERSON ( 'NAUO-PER32', 'UNSPECIFIED', 'UNSPECIFIED', ('UNSPECIFIED'), ('UNSPECIFIED'), ('UNSPECIFIED') ) ;
#22643 = COORDINATED_UNIVERSAL_TIME_OFFSET ( 0, 0, .AHEAD. ) ;
#22644 = VECTOR ( 'NONE', #22684, 1000.000000000000000 ) ;
#22645 = DIRECTION ( 'NONE',  ( -1.239096229992445915E-15, -4.969341027244109908E-15, -1.000000000000000000 ) ) ;
#22646 = AXIS2_PLACEMENT_3D ( 'NONE', #18966, #6371, #4941 ) ;
#22647 = CONICAL_SURFACE ( 'NONE', #18109, 2.254620000000000513, 0.7853981633974461696 ) ;
#22648 = AXIS2_PLACEMENT_3D ( 'NONE', #15340, #19028, #4414 ) ;
#22649 = CARTESIAN_POINT ( 'NONE',  ( -65.82868329340040248, -8.344790992841081945, -5.895754578401062139E-15 ) ) ;
#22650 = ORIENTED_EDGE ( 'NONE', *, *, #5000, .F. ) ;
#22651 = EDGE_CURVE ( 'NONE', #13977, #12003, #7885, .T. ) ;
#22652 = APPLICATION_PROTOCOL_DEFINITION ( 'international standard', 'config_control_design', 1994, #14278 ) ;
#22653 = ORIENTED_EDGE ( 'NONE', *, *, #22294, .F. ) ;
#22654 = AXIS2_PLACEMENT_3D ( 'NONE', #11147, #15024, #9458 ) ;
#22655 = LINE ( 'NONE', #1036, #15617 ) ;
#22656 = CARTESIAN_POINT ( 'NONE',  ( 52.49909637502329929, -7.592283011512620305, -13.00000000000039968 ) ) ;
#22657 = ORIENTED_EDGE ( 'NONE', *, *, #192, .T. ) ;
#22658 = DIRECTION ( 'NONE',  ( -1.000000000000000000, -6.662111140531837817E-09, 1.144917494144693313E-14 ) ) ;
#22659 = DIRECTION ( 'NONE',  ( 0.2306359803922017615, 0.9730401042858037863, -3.356987858687580135E-15 ) ) ;
#22660 = SPHERICAL_SURFACE ( 'NONE', #21350, 15.25000000000000000 ) ;
#22661 = VECTOR ( 'NONE', #11266, 999.9999999999998863 ) ;
#22662 = VERTEX_POINT ( 'NONE', #863 ) ;
#22663 = VERTEX_POINT ( 'NONE', #2779 ) ;
#22664 = DIRECTION ( 'NONE',  ( 0.000000000000000000, 1.000000000000000000, 0.000000000000000000 ) ) ;
#22665 = ORIENTED_EDGE ( 'NONE', *, *, #3611, .F. ) ;
#22666 = PERSON_AND_ORGANIZATION_ROLE ( 'classification_officer' ) ;
#22667 = VECTOR ( 'NONE', #17150, 1000.000000000000000 ) ;
#22668 = ORIENTED_EDGE ( 'NONE', *, *, #18467, .T. ) ;
#22669 = ORIENTED_EDGE ( 'NONE', *, *, #4139, .F. ) ;
#22670 = DIRECTION ( 'NONE',  ( 3.099353312215989243E-62, -1.534091707905539548E-92, -1.000000000000000000 ) ) ;
#22671 = VECTOR ( 'NONE', #4584, 1000.000000000000000 ) ;
#22672 = PERSON_AND_ORGANIZATION ( #11966, #8758 ) ;
#22673 = PERSON ( 'NAUO-PER30', 'UNSPECIFIED', 'UNSPECIFIED', ('UNSPECIFIED'), ('UNSPECIFIED'), ('UNSPECIFIED') ) ;
#22674 = DIRECTION ( 'NONE',  ( -0.1997366180463770735, -0.8426774492125654881, -0.4999999999999997780 ) ) ;
#22675 = CARTESIAN_POINT ( 'NONE',  ( -17.50000000397270128, 22.95208920922877738, 6.750000000004441780 ) ) ;
#22676 = EDGE_CURVE ( 'NONE', #12333, #19198, #4844, .T. ) ;
#22677 = APPROVAL_STATUS ( 'not_yet_approved' ) ;
#22678 = AXIS2_PLACEMENT_3D ( 'NONE', #8487, #10156, #8355 ) ;
#22679 = EDGE_LOOP ( 'NONE', ( #21553, #13247, #7952, #14963 ) ) ;
#22680 = CYLINDRICAL_SURFACE ( 'NONE', #10677, 2.500000000000001332 ) ;
#22681 = CARTESIAN_POINT ( 'NONE',  ( -65.82539143210260590, 12.65551411021120032, -5.000000000000000000 ) ) ;
#22682 = ORIENTED_EDGE ( 'NONE', *, *, #2258, .F. ) ;
#22683 = APPROVAL ( #9475, 'UNKNOWN' ) ;
#22684 = DIRECTION ( 'NONE',  ( -1.187319687680494078E-16, -2.805478249478260493E-20, -1.000000000000000000 ) ) ;
#22685 = FACE_OUTER_BOUND ( 'NONE', #7603, .T. ) ;
#22686 = EDGE_LOOP ( 'NONE', ( #4636, #8116, #4948, #18653, #8881 ) ) ;
#22687 = DIRECTION ( 'NONE',  ( -1.000000000000000000, 0.000000000000000000, 0.000000000000000000 ) ) ;
#22688 = ADVANCED_FACE ( 'NONE', ( #4786 ), #10045, .F. ) ;
#22689 = EDGE_CURVE ( 'NONE', #19560, #15573, #21148, .T. ) ;
#22690 = APPROVAL_STATUS ( 'not_yet_approved' ) ;
#22691 = ORIENTED_EDGE ( 'NONE', *, *, #7696, .T. ) ;
#22692 = ORIENTED_EDGE ( 'NONE', *, *, #2108, .T. ) ;
#22693 = FACE_BOUND ( 'NONE', #2880, .T. ) ;
#22694 = DIRECTION ( 'NONE',  ( -0.1630842657209360114, -0.6880432561069645958, -0.7071067811865398012 ) ) ;
#22695 = ORIENTED_EDGE ( 'NONE', *, *, #3323, .F. ) ;
#22696 = DATE_TIME_ROLE ( 'classification_date' ) ;
#22697 = CARTESIAN_POINT ( 'NONE',  ( 36.57467860885130051, 21.71590586959139912, 15.00000000000000000 ) ) ;
#22698 = CLOSED_SHELL ( 'NONE', ( #17619, #13696, #8797, #23251, #2547, #12619, #19707, #13784, #2214, #20332, #15868, #19306, #15557, #17279, #19250, #3805, #8978, #11846, #5458, #23170 ) ) ;
#22699 = DIRECTION ( 'NONE',  ( 0.000000000000000000, 0.000000000000000000, 1.000000000000000000 ) ) ;
#22700 = APPROVAL_ROLE ( '' ) ;
#22701 = CARTESIAN_POINT ( 'NONE',  ( 1.132413798561739802E-13, -1.842903579429180027E-16, -8.889558542813568797E-14 ) ) ;
#22702 =( NAMED_UNIT ( * ) SI_UNIT ( $, .STERADIAN. ) SOLID_ANGLE_UNIT ( ) );
#22703 = AXIS2_PLACEMENT_3D ( 'NONE', #6001, #885, #8148 ) ;
#22704 = DIRECTION ( 'NONE',  ( 0.9999862922474493931, 0.005235963827108502076, 0.000000000000000000 ) ) ;
#22705 = EDGE_CURVE ( 'NONE', #16708, #19614, #10177, .T. ) ;
#22706 = MECHANICAL_CONTEXT ( 'NONE', #3050, 'mechanical' ) ;
#22707 = DIRECTION ( 'NONE',  ( 3.338698890017581616E-19, -6.376386915953721864E-17, 1.000000000000000000 ) ) ;
#22708 = LINE ( 'NONE', #6590, #8620 ) ;
#22709 = CC_DESIGN_PERSON_AND_ORGANIZATION_ASSIGNMENT ( #15025, #16676, ( #480 ) ) ;
#22710 = FACE_OUTER_BOUND ( 'NONE', #12468, .T. ) ;
#22711 = DIRECTION ( 'NONE',  ( 0.9999862922474493931, 0.005235963827117055998, -1.750845403988397166E-31 ) ) ;
#22712 = PRODUCT_RELATED_PRODUCT_CATEGORY ( 'detail', '', ( #8325 ) ) ;
#22713 = FACE_OUTER_BOUND ( 'NONE', #22605, .T. ) ;
#22714 = DIRECTION ( 'NONE',  ( 0.000000000000000000, 1.000000000000000000, 0.000000000000000000 ) ) ;
#22715 = EDGE_CURVE ( 'NONE', #23250, #17339, #11321, .T. ) ;
#22717 = ORIENTED_EDGE ( 'NONE', *, *, #11258, .F. ) ;
#22716 = ADVANCED_FACE ( 'NONE', ( #732 ), #11949, .T. ) ;
#22718 = PRODUCT_DEFINITION_SHAPE ( 'NONE', 'NONE',  #19382 ) ;
#22719 = CC_DESIGN_PERSON_AND_ORGANIZATION_ASSIGNMENT ( #5820, #3671, ( #1978 ) ) ;
#22720 = VERTEX_POINT ( 'NONE', #12168 ) ;
#22721 = DIRECTION ( 'NONE',  ( 0.2306359803922084506, 0.9730401042858022320, -5.112869192352694760E-15 ) ) ;
#22722 = PLANE ( 'NONE',  #22703 ) ;
#22723 = LINE ( 'NONE', #5909, #15210 ) ;
#22724 = ORIENTED_EDGE ( 'NONE', *, *, #9702, .F. ) ;
#22725 = VECTOR ( 'NONE', #1814, 1000.000000000000000 ) ;
#22726 = DIRECTION ( 'NONE',  ( -0.9730401042858036753, 0.2306359803922028995, 5.959266323858677443E-17 ) ) ;
#22727 = ORIENTED_EDGE ( 'NONE', *, *, #17910, .T. ) ;
#22728 = DIRECTION ( 'NONE',  ( 6.124378941434239724E-17, -2.274246353359159970E-33, 1.000000000000000000 ) ) ;
#22729 = PERSON_AND_ORGANIZATION ( #11966, #8758 ) ;
#22730 = LINE ( 'NONE', #20842, #21111 ) ;
#22731 = COORDINATED_UNIVERSAL_TIME_OFFSET ( 0, 0, .AHEAD. ) ;
#22732 = CARTESIAN_POINT ( 'NONE',  ( 32.96699026062353255, 10.39752682851250398, 26.29999999999999716 ) ) ;
#22733 = CARTESIAN_POINT ( 'NONE',  ( -59.85533902005759899, -24.86725927682059734, 5.000000000000000000 ) ) ;
#22734 = EDGE_CURVE ( 'NONE', #9474, #21838, #9137, .T. ) ;
#22735 = CARTESIAN_POINT ( 'NONE',  ( 0.000000000000000000, 0.000000000000000000, 0.000000000000000000 ) ) ;
#22736 = CONICAL_SURFACE ( 'NONE', #6066, 2.283500000000000529, 0.7853981633974469467 ) ;
#22737 =( GEOMETRIC_REPRESENTATION_CONTEXT ( 3 ) GLOBAL_UNCERTAINTY_ASSIGNED_CONTEXT ( ( #20097 ) ) GLOBAL_UNIT_ASSIGNED_CONTEXT ( ( #2396, #1909, #9168 ) ) REPRESENTATION_CONTEXT ( 'NONE', 'WORKASPACE' ) );
#22738 = CARTESIAN_POINT ( 'NONE',  ( -22.50000000000000000, -20.00000000000000000, 2.500000000000000000 ) ) ;
#22739 = CIRCLE ( 'NONE', #13282, 2.499999999999998668 ) ;
#22740 = VERTEX_POINT ( 'NONE', #18412 ) ;
#22741 = DIRECTION ( 'NONE',  ( -8.623081276789554834E-17, -1.054188326053478339E-16, -1.000000000000000000 ) ) ;
#22742 = EDGE_CURVE ( 'NONE', #11832, #5242, #19261, .T. ) ;
#22743 = DESIGN_CONTEXT ( 'detailed design', #2331, 'design' ) ;
#22744 = CARTESIAN_POINT ( 'NONE',  ( 42.53512288715421619, 17.37899071806551277, -2.604523473037073991E-15 ) ) ;
#22745 = ORIENTED_EDGE ( 'NONE', *, *, #9260, .T. ) ;
#22746 = LINE ( 'NONE', #4715, #10532 ) ;
#22747 = DIRECTION ( 'NONE',  ( -0.9730401042858022320, 0.2306359803922080343, 5.959266323858941219E-17 ) ) ;
#22748 = AXIS2_PLACEMENT_3D ( 'NONE', #17852, #16520, #5372 ) ;
#22749 = EDGE_CURVE ( 'NONE', #15954, #1462, #21165, .T. ) ;
#22750 = APPROVAL_STATUS ( 'not_yet_approved' ) ;
#22751 = ADVANCED_FACE ( 'NONE', ( #12820 ), #12710, .F. ) ;
#22752 = LINE ( 'NONE', #13745, #6538 ) ;
#22753 =( BOUNDED_CURVE ( )  B_SPLINE_CURVE ( 2, ( #1826, #16206, #16096 ),
 .UNSPECIFIED., .F., .F. ) 
 B_SPLINE_CURVE_WITH_KNOTS ( ( 3, 3 ),
 ( 0.08763271035584145607, 0.1752654207116860208 ),
 .UNSPECIFIED. ) 
 CURVE ( )  GEOMETRIC_REPRESENTATION_ITEM ( )  RATIONAL_B_SPLINE_CURVE ( ( 1.077350269189624843, 1.077350269189626175, 1.000000000000000000 ) ) 
 REPRESENTATION_ITEM ( '' )  );
#22754 = ORIENTED_EDGE ( 'NONE', *, *, #16840, .F. ) ;
#22755 = ORIENTED_EDGE ( 'NONE', *, *, #14610, .F. ) ;
#22756 = MECHANICAL_CONTEXT ( 'NONE', #16400, 'mechanical' ) ;
#22757 = DIRECTION ( 'NONE',  ( -0.8823529412199823119, 0.4705882352125332901, 8.962737959213505425E-15 ) ) ;
#22758 = ORIENTED_EDGE ( 'NONE', *, *, #9512, .T. ) ;
#22759 = CC_DESIGN_SECURITY_CLASSIFICATION ( #7977, ( #1510 ) ) ;
#22760 = CARTESIAN_POINT ( 'NONE',  ( -17.50000000000000000, -20.00000000000000000, 7.748383280539972460E-62 ) ) ;
#22761 = CALENDAR_DATE ( 2026, 31, 10 ) ;
#22762 = COORDINATED_UNIVERSAL_TIME_OFFSET ( 0, 0, .AHEAD. ) ;
#22763 = DIRECTION ( 'NONE',  ( -1.138590270679731958E-14, -2.220446049251245514E-15, -1.000000000000000000 ) ) ;
#22764 = AXIS2_PLACEMENT_3D ( 'NONE', #6490, #18621, #4118 ) ;
#22765 = VECTOR ( 'NONE', #14270, 999.9999999999998863 ) ;
#22766 = FACE_OUTER_BOUND ( 'NONE', #20421, .T. ) ;
#22767 = ORIENTED_EDGE ( 'NONE', *, *, #20053, .T. ) ;
#22768 = COORDINATED_UNIVERSAL_TIME_OFFSET ( 0, 0, .AHEAD. ) ;
#22769 = LOCAL_TIME ( 14, 11, 27.00000000000000000, #12385 ) ;
#22770 = ORIENTED_EDGE ( 'NONE', *, *, #20721, .F. ) ;
#22771 = APPROVAL_PERSON_ORGANIZATION ( #17628, #18024, #10273 ) ;
#22772 = DIRECTION ( 'NONE',  ( 1.159535895544890222E-14, 2.167612681253619929E-15, 1.000000000000000000 ) ) ;
#22773 = LINE ( 'NONE', #22427, #5551 ) ;
#22774 = ORIENTED_EDGE ( 'NONE', *, *, #15298, .F. ) ;
#22775 = EDGE_CURVE ( 'NONE', #12473, #1257, #21430, .T. ) ;
#22776 = AXIS2_PLACEMENT_3D ( 'NONE', #21446, #1131, #8398 ) ;
#22777 = CARTESIAN_POINT ( 'NONE',  ( 61.45890873801150178, 17.00438549795339682, 13.00000000000000000 ) ) ;
#22778 = SECURITY_CLASSIFICATION ( '', '', #15639 ) ;
#22779 = DIRECTION ( 'NONE',  ( -0.9999863470142589250, -0.005225493764064552404, 0.000000000000000000 ) ) ;
#22780 = DIRECTION ( 'NONE',  ( -0.9997651245102160411, -0.02167246670483411256, 0.000000000000000000 ) ) ;
#22781 = EDGE_LOOP ( 'NONE', ( #14292, #10474, #19545, #17369, #15137, #14237, #1474, #22333, #10010, #7996, #17364, #1350, #9093, #8657, #20066, #19556, #1368, #14535, #17162, #17404, #13644, #15144, #424, #21025, #14819, #14698, #2756, #147, #18149, #12751, #11046, #5308, #23470, #18446, #14259, #8463, #12779, #16997, #12247, #20153, #3192, #13310, #14983, #14959, #22551, #11581, #22959, #18846 ) ) ;
#22782 = ORIENTED_EDGE ( 'NONE', *, *, #7412, .F. ) ;
#22783 = CARTESIAN_POINT ( 'NONE',  ( -16.50082286259682363, 23.02797946379152094, -3.750000000000000000 ) ) ;
#22784 = EDGE_LOOP ( 'NONE', ( #15807, #7414 ) ) ;
#22785 = CIRCLE ( 'NONE', #2313, 6.000000000000000000 ) ;
#22786 = DATE_AND_TIME ( #12248, #776 ) ;
#22787 = ORIENTED_EDGE ( 'NONE', *, *, #13270, .F. ) ;
#22788 = EDGE_LOOP ( 'NONE', ( #22548, #18181, #19727, #15281 ) ) ;
#22789 = PLANE ( 'NONE',  #4273 ) ;
#22790 = APPLICATION_PROTOCOL_DEFINITION ( 'international standard', 'config_control_design', 1994, #7911 ) ;
#22791 = ADVANCED_FACE ( 'NONE', ( #3564 ), #12597, .T. ) ;
#22792 = APPROVAL_PERSON_ORGANIZATION ( #20290, #17220, #4014 ) ;
#22793 = DIRECTION ( 'NONE',  ( 0.000000000000000000, 0.000000000000000000, -1.000000000000000000 ) ) ;
#22794 = LOCAL_TIME ( 14, 11, 27.00000000000000000, #8212 ) ;
#22795 = CC_DESIGN_APPROVAL ( #12270, ( #1162 ) ) ;
#22796 = DIRECTION ( 'NONE',  ( 0.000000000000000000, 0.000000000000000000, 1.000000000000000000 ) ) ;
#22797 = SECURITY_CLASSIFICATION ( '', '', #9339 ) ;
#22798 = DIRECTION ( 'NONE',  ( -0.9730401042858035643, 0.2306359803922028717, 5.958148513035547083E-17 ) ) ;
#22799 = FACE_OUTER_BOUND ( 'NONE', #6209, .T. ) ;
#22800 = CALENDAR_DATE ( 2026, 31, 10 ) ;
#22801 = ORIENTED_EDGE ( 'NONE', *, *, #12571, .T. ) ;
#22802 = DIRECTION ( 'NONE',  ( 0.9730401042858020100, -0.2306359803922089780, 0.000000000000000000 ) ) ;
#22803 = DIRECTION ( 'NONE',  ( -6.123237831918399306E-17, 1.569224110909209817E-30, 1.000000000000000000 ) ) ;
#22804 = EDGE_LOOP ( 'NONE', ( #9483, #9270, #12923, #3491, #18277, #8961, #20516, #17314 ) ) ;
#22805 = CC_DESIGN_APPROVAL ( #16184, ( #795 ) ) ;
#22806 = CARTESIAN_POINT ( 'NONE',  ( -56.98461483124570037, -21.79876819407909849, -1.072991366992009803E-14 ) ) ;
#22807 = DIRECTION ( 'NONE',  ( 2.269747459788994803E-13, 2.220446049250330436E-15, 1.000000000000000000 ) ) ;
#22808 = DIRECTION ( 'NONE',  ( 1.000000000000000000, 0.000000000000000000, 0.000000000000000000 ) ) ;
#22809 = ORIENTED_EDGE ( 'NONE', *, *, #5201, .F. ) ;
#22810 = DIRECTION ( 'NONE',  ( 3.469446951953605354E-14, 9.757819552369514663E-14, -1.000000000000000000 ) ) ;
#22811 = VECTOR ( 'NONE', #21226, 999.9999999999998863 ) ;
#22812 = CALENDAR_DATE ( 2026, 31, 10 ) ;
#22813 = ORIENTED_EDGE ( 'NONE', *, *, #6201, .F. ) ;
#22814 = VERTEX_POINT ( 'NONE', #3908 ) ;
#22815 = LINE ( 'NONE', #8227, #5430 ) ;
#22816 = CARTESIAN_POINT ( 'NONE',  ( -68.70795112897079093, 11.84741790582710053, 3.773156417642989929E-15 ) ) ;
#22817 = LOCAL_TIME ( 14, 11, 27.00000000000000000, #15744 ) ;
#22818 = ORIENTED_EDGE ( 'NONE', *, *, #15135, .T. ) ;
#22819 = DATE_AND_TIME ( #15714, #11489 ) ;
#22820 = EDGE_CURVE ( 'NONE', #1137, #5883, #12352, .T. ) ;
#22821 = DIRECTION ( 'NONE',  ( -0.8660135325225011282, -0.004534477687572233823, 0.5000000000000000000 ) ) ;
#22822 = EDGE_CURVE ( 'NONE', #15508, #22078, #16119, .T. ) ;
#22823 = DIRECTION ( 'NONE',  ( 0.2306359803922030938, 0.9730401042858035643, -4.741332172907964454E-18 ) ) ;
#22824 = COORDINATED_UNIVERSAL_TIME_OFFSET ( 0, 0, .AHEAD. ) ;
#22825 = CARTESIAN_POINT ( 'NONE',  ( 114.8178196092480050, -22.36345201740219935, 13.00000000000000000 ) ) ;
#22826 = APPROVAL_PERSON_ORGANIZATION ( #15932, #18376, #10262 ) ;
#22827 = ADVANCED_FACE ( 'NONE', ( #20052 ), #5457, .F. ) ;
#22828 = AXIS2_PLACEMENT_3D ( 'NONE', #20171, #7358, #1866 ) ;
#22829 = EDGE_CURVE ( 'NONE', #15338, #7111, #16372, .T. ) ;
#22830 = CARTESIAN_POINT ( 'NONE',  ( -62.73971250800079957, -25.32895006819559924, 5.000000000000000000 ) ) ;
#22831 = APPROVAL_ROLE ( '' ) ;
#22832 = AXIS2_PLACEMENT_3D ( 'NONE', #5084, #13868, #21100 ) ;
#22833 = VECTOR ( 'NONE', #1836, 999.9999999999998863 ) ;
#22834 = ORGANIZATION ( 'NAUO-ORG35', 'UNSPECIFIED', 'UNSPECIFIED' ) ;
#22835 = DIRECTION ( 'NONE',  ( 3.210834492181045054E-17, -2.441916418604795262E-15, -1.000000000000000000 ) ) ;
#22836 = CARTESIAN_POINT ( 'NONE',  ( 120.0770346556423931, 0.7635863056469011090, -13.00000000000000000 ) ) ;
#22837 = AXIS2_PLACEMENT_3D ( 'NONE', #20802, #10378, #4531 ) ;
#22838 = CARTESIAN_POINT ( 'NONE',  ( 118.4388045014059969, -7.086722380115170417, -18.89999999999999858 ) ) ;
#22839 = CARTESIAN_POINT ( 'NONE',  ( -62.91249983789198552, 7.670697574599230073, 2.108981951733699973E-15 ) ) ;
#22840 = CIRCLE ( 'NONE', #451, 2.500000000000000444 ) ;
#22841 = CARTESIAN_POINT ( 'NONE',  ( 2.500000000000000000, 3.061616997868383141E-16, -5.000000000000000000 ) ) ;
#22842 = ORIENTED_EDGE ( 'NONE', *, *, #8270, .F. ) ;
#22843 = CARTESIAN_POINT ( 'NONE',  ( -62.93704341833160498, 12.35813331950920002, 3.344713564077609812E-15 ) ) ;
#22844 = VERTEX_POINT ( 'NONE', #14043 ) ;
#22845 = CC_DESIGN_SECURITY_CLASSIFICATION ( #6551, ( #1997 ) ) ;
#22846 = VERTEX_POINT ( 'NONE', #13930 ) ;
#22847 = CARTESIAN_POINT ( 'NONE',  ( -14.00000000202730099, 1.899127378930349996, -7.999999999996879829 ) ) ;
#22848 = DIRECTION ( 'NONE',  ( -1.187319687680499994E-16, -2.805478249478640262E-20, -1.000000000000000000 ) ) ;
#22849 = ORIENTED_EDGE ( 'NONE', *, *, #18961, .F. ) ;
#22850 = VECTOR ( 'NONE', #14495, 1000.000000000000000 ) ;
#22851 = AXIS2_PLACEMENT_3D ( 'NONE', #15018, #9706, #884 ) ;
#22852 = DIRECTION ( 'NONE',  ( 0.1997366180463766849, 0.8426774492125652660, -0.5000000000000004441 ) ) ;
#22853 = ADVANCED_FACE ( 'NONE', ( #5563 ), #8593, .F. ) ;
#22854 = ORIENTED_EDGE ( 'NONE', *, *, #15524, .F. ) ;
#22855 = AXIS2_PLACEMENT_3D ( 'NONE', #20722, #11727, #6356 ) ;
#22856 = CARTESIAN_POINT ( 'NONE',  ( -19.80660126203780180, 15.09635365252939998, 2.500000000000000000 ) ) ;
#22857 = PERSON_AND_ORGANIZATION ( #11966, #8758 ) ;
#22858 = CARTESIAN_POINT ( 'NONE',  ( 35.94015251278350576, 11.23436983788223209, 27.55602540378454179 ) ) ;
#22859 = CC_DESIGN_PERSON_AND_ORGANIZATION_ASSIGNMENT ( #17870, #9073, ( #15182 ) ) ;
#22860 = CC_DESIGN_PERSON_AND_ORGANIZATION_ASSIGNMENT ( #21274, #10615, ( #3492 ) ) ;
#22861 = CALENDAR_DATE ( 2026, 31, 10 ) ;
#22862 = CIRCLE ( 'NONE', #12645, 1.000000000000000888 ) ;
#22864 = FACE_OUTER_BOUND ( 'NONE', #23101, .T. ) ;
#22863 = CIRCLE ( 'NONE', #3529, 2.500000000000000444 ) ;
#22865 = EDGE_CURVE ( 'NONE', #9929, #22253, #9027, .T. ) ;
#22866 = EDGE_CURVE ( 'NONE', #13843, #5040, #21717, .T. ) ;
#22867 = CARTESIAN_POINT ( 'NONE',  ( -14.00000000144740042, -4.350228928435730502, 6.750000000004459544 ) ) ;
#22868 = APPROVAL_PERSON_ORGANIZATION ( #20726, #651, #17525 ) ;
#22869 = DIRECTION ( 'NONE',  ( 0.9730401042858035643, -0.2306359803922031215, 2.804983810440351899E-16 ) ) ;
#22870 = AXIS2_PLACEMENT_3D ( 'NONE', #12121, #20773, #19001 ) ;
#22871 = ORIENTED_EDGE ( 'NONE', *, *, #3012, .F. ) ;
#22872 = LINE ( 'NONE', #13734, #7496 ) ;
#22873 = AXIS2_PLACEMENT_3D ( 'NONE', #11469, #22122, #17135 ) ;
#22874 = CARTESIAN_POINT ( 'NONE',  ( -19.55420733641118147, 2.397309549614579982, -2.500000000000006217 ) ) ;
#22875 = ORIENTED_EDGE ( 'NONE', *, *, #108, .T. ) ;
#22876 = CARTESIAN_POINT ( 'NONE',  ( 35.39632699307497177, 11.83676830303470240, -8.783982963266950605 ) ) ;
#22877 = CARTESIAN_POINT ( 'NONE',  ( 114.8178196092480050, -22.36345201740219935, -13.00000000000000000 ) ) ;
#22878 = COORDINATED_UNIVERSAL_TIME_OFFSET ( 0, 0, .AHEAD. ) ;
#22879 = FACE_OUTER_BOUND ( 'NONE', #7345, .T. ) ;
#22880 = EDGE_LOOP ( 'NONE', ( #16302, #16570, #81, #15348 ) ) ;
#22881 = CIRCLE ( 'NONE', #16054, 2.500000000000000444 ) ;
#22882 = VERTEX_POINT ( 'NONE', #14599 ) ;
#22883 = CALENDAR_DATE ( 2026, 31, 10 ) ;
#22884 = CARTESIAN_POINT ( 'NONE',  ( 114.8178196092480050, -22.36345201740209987, 20.00000000000000000 ) ) ;
#22885 = EDGE_CURVE ( 'NONE', #2801, #3556, #18408, .T. ) ;
#22886 = SECURITY_CLASSIFICATION ( '', '', #4434 ) ;
#22887 = CIRCLE ( 'NONE', #16820, 2.500000000000001776 ) ;
#22888 = ORIENTED_EDGE ( 'NONE', *, *, #1657, .F. ) ;
#22889 = FACE_OUTER_BOUND ( 'NONE', #6006, .T. ) ;
#22890 = PERSON_AND_ORGANIZATION ( #11966, #8758 ) ;
#22891 = CIRCLE ( 'NONE', #8103, 5.999999999999999112 ) ;
#22892 = AXIS2_PLACEMENT_3D ( 'NONE', #20835, #14468, #12699 ) ;
#22893 = APPROVAL_DATE_TIME ( #10091, #23407 ) ;
#22894 = DIRECTION ( 'NONE',  ( -1.466984912809907930E-16, -2.805478249466190329E-20, -1.000000000000000000 ) ) ;
#22895 = EDGE_CURVE ( 'NONE', #17258, #16156, #21829, .T. ) ;
#22896 = EDGE_CURVE ( 'NONE', #17221, #16018, #7475, .T. ) ;
#22897 = LINE ( 'NONE', #6511, #3181 ) ;
#22898 = ORIENTED_EDGE ( 'NONE', *, *, #94, .T. ) ;
#22899 = AXIS2_PLACEMENT_3D ( 'NONE', #12329, #13732, #1004 ) ;
#22900 = VERTEX_POINT ( 'NONE', #12929 ) ;
#22901 = VECTOR ( 'NONE', #18424, 1000.000000000000227 ) ;
#22902 = DIRECTION ( 'NONE',  ( -0.9730401042858024541, 0.2306359803922080898, 5.959266323858862332E-17 ) ) ;
#22903 = FACE_BOUND ( 'NONE', #20693, .T. ) ;
#22904 = ORIENTED_EDGE ( 'NONE', *, *, #4585, .T. ) ;
#22905 = DIRECTION ( 'NONE',  ( -6.662112528310618598E-09, 1.000000000000000000, -2.081668171172169697E-15 ) ) ;
#22906 = DIRECTION ( 'NONE',  ( 0.9730401042858035643, -0.2306359803922028717, 2.025546614365803772E-16 ) ) ;
#22907 = EDGE_LOOP ( 'NONE', ( #8219, #23076 ) ) ;
#22908 = ORIENTED_EDGE ( 'NONE', *, *, #5345, .F. ) ;
#22909 = DIRECTION ( 'NONE',  ( -0.2306359803922080343, -0.9730401042858022320, -3.574477303645861237E-15 ) ) ;
#22910 = ORIENTED_EDGE ( 'NONE', *, *, #5626, .T. ) ;
#22911 = PERSON_AND_ORGANIZATION ( #11966, #8758 ) ;
#22912 = EDGE_CURVE ( 'NONE', #2044, #18542, #20298, .T. ) ;
#22913 = ORIENTED_EDGE ( 'NONE', *, *, #3617, .T. ) ;
#22914 = ORIENTED_EDGE ( 'NONE', *, *, #18221, .T. ) ;
#22915 = CARTESIAN_POINT ( 'NONE',  ( 30.84445860938240003, -2.459566909556570202, 13.00000000000019895 ) ) ;
#22916 = DATE_AND_TIME ( #19144, #8041 ) ;
#22917 = CARTESIAN_POINT ( 'NONE',  ( 96.81657767996070163, -18.09668638014640152, -13.00000000000000000 ) ) ;
#22918 = APPLICATION_CONTEXT ( 'configuration controlled 3d designs of mechanical parts and assemblies' ) ;
#22919 = EDGE_CURVE ( 'NONE', #18542, #2044, #11217, .T. ) ;
#22920 = EDGE_CURVE ( 'NONE', #1142, #12006, #22178, .T. ) ;
#22921 = CARTESIAN_POINT ( 'NONE',  ( 45.07211867146960316, 28.08243186520980217, 10.02499999999999858 ) ) ;
#22922 = CARTESIAN_POINT ( 'NONE',  ( 35.59419854219520118, 9.774809681453278998, 25.00000000000000000 ) ) ;
#22923 = COORDINATED_UNIVERSAL_TIME_OFFSET ( 0, 0, .AHEAD. ) ;
#22924 = PRODUCT_DEFINITION_SHAPE ( 'NONE', 'NONE',  #12089 ) ;
#22925 = ORIENTED_EDGE ( 'NONE', *, *, #19403, .F. ) ;
#22926 = DIRECTION ( 'NONE',  ( 0.9730401042858036753, -0.2306359803922028995, -5.959266323858677443E-17 ) ) ;
#22927 = ORIENTED_EDGE ( 'NONE', *, *, #22234, .T. ) ;
#22928 = CARTESIAN_POINT ( 'NONE',  ( -69.91240388362379576, 7.634045827809347706, 7.200000000000000178 ) ) ;
#22929 = DIRECTION ( 'NONE',  ( 0.9730401042858035643, -0.2306359803922028717, 2.740969466505750030E-16 ) ) ;
#22930 = CARTESIAN_POINT ( 'NONE',  ( -20.00000000397129796, 22.95208919256900160, -8.749999999995699440 ) ) ;
#22931 = ORIENTED_EDGE ( 'NONE', *, *, #11286, .F. ) ;
#22932 = DIRECTION ( 'NONE',  ( -0.9730401042858024541, 0.2306359803922080898, 5.959266323858942451E-17 ) ) ;
#22933 = AXIS2_PLACEMENT_3D ( 'NONE', #18312, #5701, #14848 ) ;
#22934 = APPROVAL_STATUS ( 'not_yet_approved' ) ;
#22935 = VERTEX_POINT ( 'NONE', #9850 ) ;
#22936 = ORIENTED_EDGE ( 'NONE', *, *, #21539, .T. ) ;
#22937 = DIRECTION ( 'NONE',  ( -1.000000000000000000, -6.662112528310618598E-09, 2.269018306577664942E-13 ) ) ;
#22938 = CARTESIAN_POINT ( 'NONE',  ( -26.00000000000000000, -20.00000000055539928, 8.000000000004630962 ) ) ;
#22939 = CARTESIAN_POINT ( 'NONE',  ( 35.93893384793820189, -10.44995626450799975, -3.100000000000000089 ) ) ;
#22940 = DATE_TIME_ROLE ( 'creation_date' ) ;
#22941 = CC_DESIGN_DATE_AND_TIME_ASSIGNMENT ( #2067, #17145, ( #7616 ) ) ;
#22942 = LINE ( 'NONE', #23054, #4681 ) ;
#22943 = CARTESIAN_POINT ( 'NONE',  ( 35.34171762861025456, 30.38879166913039853, -20.00000000000029843 ) ) ;
#22944 = DIRECTION ( 'NONE',  ( -2.269747459788994803E-13, -2.220446049250320181E-15, -1.000000000000000000 ) ) ;
#22945 = ADVANCED_BREP_SHAPE_REPRESENTATION ( '', ( #9573, #12739 ), #3033 ) ;
#22946 = AXIS2_PLACEMENT_3D ( 'NONE', #6645, #13634, #11884 ) ;
#22947 = CARTESIAN_POINT ( 'NONE',  ( -19.44579266323601985, -2.601514938066536331, -4.999999999999993783 ) ) ;
#22948 = DATE_AND_TIME ( #13581, #16352 ) ;
#22949 = DIRECTION ( 'NONE',  ( -0.2306359803922088947, -0.9730401042858021210, 5.139921410301650007E-15 ) ) ;
#22950 = DIRECTION ( 'NONE',  ( 0.000000000000000000, 0.000000000000000000, 1.000000000000000000 ) ) ;
#22951 = CARTESIAN_POINT ( 'NONE',  ( 102.8131131701580046, 7.202356331284469171, -13.00000000000000000 ) ) ;
#22952 = EDGE_CURVE ( 'NONE', #990, #16449, #2598, .T. ) ;
#22953 = CARTESIAN_POINT ( 'NONE',  ( 118.5310588935630136, -6.697506338400800452, -20.00000000000000000 ) ) ;
#22954 = DIRECTION ( 'NONE',  ( 0.7273594590164640383, -0.6862566701892790499, 3.364551046996709526E-15 ) ) ;
#22955 = ORIENTED_EDGE ( 'NONE', *, *, #17193, .F. ) ;
#22956 = APPLICATION_CONTEXT ( 'configuration controlled 3d designs of mechanical parts and assemblies' ) ;
#22957 = LINE ( 'NONE', #4800, #8842 ) ;
#22958 = VERTEX_POINT ( 'NONE', #6155 ) ;
#22959 = ORIENTED_EDGE ( 'NONE', *, *, #17179, .F. ) ;
#22960 = DIRECTION ( 'NONE',  ( -3.099353312215988811E-62, 0.000000000000000000, 1.000000000000000000 ) ) ;
#22961 = SHAPE_REPRESENTATION ( 'Pin', ( #12739 ), #14020 ) ;
#22962 = PLANE ( 'NONE',  #4905 ) ;
#22963 = ORIENTED_EDGE ( 'NONE', *, *, #5316, .T. ) ;
#22964 = CARTESIAN_POINT ( 'NONE',  ( -4.514225866272970400, 4.676725866273559795, -2.500000000000000000 ) ) ;
#22965 = ORIENTED_EDGE ( 'NONE', *, *, #9853, .F. ) ;
#22966 = LINE ( 'NONE', #22509, #10637 ) ;
#22967 = APPROVAL_ROLE ( '' ) ;
#22968 = DIRECTION ( 'NONE',  ( -1.000000000000000000, 0.000000000000000000, 0.000000000000000000 ) ) ;
#22969 = CONTEXT_DEPENDENT_SHAPE_REPRESENTATION ( #1101, #9497 ) ;
#22970 = DIRECTION ( 'NONE',  ( 1.000000000000000000, 0.000000000000000000, 0.000000000000000000 ) ) ;
#22971 = DIRECTION ( 'NONE',  ( 0.9730401042858026761, -0.2306359803922063967, 0.000000000000000000 ) ) ;
#22972 = DIRECTION ( 'NONE',  ( -1.000000000000000000, 2.270069654138870255E-15, -3.099353312215989243E-62 ) ) ;
#22973 = DIRECTION ( 'NONE',  ( 2.269747459788999852E-13, 2.220446049250325308E-15, 1.000000000000000000 ) ) ;
#22974 = ORIENTED_EDGE ( 'NONE', *, *, #12359, .F. ) ;
#22975 = DIRECTION ( 'NONE',  ( -0.9730401042858024541, 0.2306359803922080898, 5.959266323858942451E-17 ) ) ;
#22976 = AXIS2_PLACEMENT_3D ( 'NONE', #6191, #16870, #2862 ) ;
#22977 = EDGE_CURVE ( 'NONE', #7436, #8698, #16960, .T. ) ;
#22978 = DESIGN_CONTEXT ( 'detailed design', #3996, 'design' ) ;
#22979 = ORIENTED_EDGE ( 'NONE', *, *, #17837, .T. ) ;
#22980 = CARTESIAN_POINT ( 'NONE',  ( 33.52368772877015601, 9.713198297474395559, -8.984918777770040776 ) ) ;
#22981 = DIRECTION ( 'NONE',  ( 0.7071067811865475727, 0.000000000000000000, -0.7071067811865474617 ) ) ;
#22982 = CC_DESIGN_DATE_AND_TIME_ASSIGNMENT ( #7356, #18155, ( #17552 ) ) ;
#22983 = ORIENTED_EDGE ( 'NONE', *, *, #20877, .T. ) ;
#22984 = COORDINATED_UNIVERSAL_TIME_OFFSET ( 0, 0, .AHEAD. ) ;
#22985 = DIRECTION ( 'NONE',  ( -0.9730401042858035643, 0.2306359803922028717, 5.959266323858679908E-17 ) ) ;
#22986 = ORIENTED_EDGE ( 'NONE', *, *, #14908, .T. ) ;
#22987 = ORIENTED_EDGE ( 'NONE', *, *, #14164, .T. ) ;
#22988 = EDGE_CURVE ( 'NONE', #16977, #115, #20677, .T. ) ;
#22989 = EDGE_CURVE ( 'NONE', #12945, #5544, #19533, .T. ) ;
#22990 = PERSON_AND_ORGANIZATION_ROLE ( 'design_owner' ) ;
#22991 = DIRECTION ( 'NONE',  ( 0.000000000000000000, -1.000000000000000000, 0.000000000000000000 ) ) ;
#22992 = ORIENTED_EDGE ( 'NONE', *, *, #3160, .F. ) ;
#22993 = AXIS2_PLACEMENT_3D ( 'NONE', #20037, #10808, #9009 ) ;
#22994 = VECTOR ( 'NONE', #9921, 1000.000000000000000 ) ;
#22995 = DIRECTION ( 'NONE',  ( -0.9286452767786568252, -1.871119812896369614E-17, -0.3709689338970204586 ) ) ;
#22996 = APPROVAL_STATUS ( 'not_yet_approved' ) ;
#22997 = APPROVAL_DATE_TIME ( #1386, #4117 ) ;
#22998 = CARTESIAN_POINT ( 'NONE',  ( -19.49999999982360066, -0.1021026942259809916, -5.000000000000000000 ) ) ;
#22999 = CARTESIAN_POINT ( 'NONE',  ( 50.90756547144189881, 18.01515514085709668, 3.544128957608909560E-14 ) ) ;
#23000 = EDGE_LOOP ( 'NONE', ( #9737, #4693, #5227, #21729, #8533 ) ) ;
#23001 = EDGE_CURVE ( 'NONE', #17831, #17030, #6664, .T. ) ;
#23002 = VECTOR ( 'NONE', #22032, 1000.000000000000000 ) ;
#23003 = CONICAL_SURFACE ( 'NONE', #22239, 2.254620000000000513, 0.7853981633974461696 ) ;
#23004 = CIRCLE ( 'NONE', #20357, 0.4000000000000001887 ) ;
#23005 = ORIENTED_EDGE ( 'NONE', *, *, #2072, .F. ) ;
#23006 = CARTESIAN_POINT ( 'NONE',  ( -2.500000000000000000, -17.30000000000000071, -2.500000000000000000 ) ) ;
#23007 = FACE_OUTER_BOUND ( 'NONE', #3258, .T. ) ;
#23008 = VERTEX_POINT ( 'NONE', #4137 ) ;
#23009 = CC_DESIGN_PERSON_AND_ORGANIZATION_ASSIGNMENT ( #201, #7470, ( #8830 ) ) ;
#23010 = CC_DESIGN_PERSON_AND_ORGANIZATION_ASSIGNMENT ( #18789, #4040, ( #13468 ) ) ;
#23011 = DIRECTION ( 'NONE',  ( 0.000000000000000000, -1.000000000000000000, 0.000000000000000000 ) ) ;
#23012 = CARTESIAN_POINT ( 'NONE',  ( 35.59419854219520118, 9.774809681453278998, -26.88000000000049994 ) ) ;
#23013 = ORIENTED_EDGE ( 'NONE', *, *, #12845, .F. ) ;
#23014 = ORIENTED_EDGE ( 'NONE', *, *, #5053, .T. ) ;
#23015 = LINE ( 'NONE', #4980, #17824 ) ;
#23016 = ORIENTED_EDGE ( 'NONE', *, *, #11909, .F. ) ;
#23017 = EDGE_CURVE ( 'NONE', #9785, #3254, #23319, .T. ) ;
#23018 = EDGE_CURVE ( 'NONE', #19719, #18548, #20300, .T. ) ;
#23019 = DATE_AND_TIME ( #10007, #7267 ) ;
#23020 = ORIENTED_EDGE ( 'NONE', *, *, #7454, .F. ) ;
#23021 = ORIENTED_EDGE ( 'NONE', *, *, #15824, .F. ) ;
#23022 = PRODUCT_RELATED_PRODUCT_CATEGORY ( 'detail', '', ( #15527 ) ) ;
#23023 = FACE_OUTER_BOUND ( 'NONE', #22, .T. ) ;
#23024 = CIRCLE ( 'NONE', #8631, 4.399999999999997691 ) ;
#23025 = PERSON_AND_ORGANIZATION ( #11966, #8758 ) ;
#23026 = AXIS2_PLACEMENT_3D ( 'NONE', #2627, #22452, #15694 ) ;
#23027 = CIRCLE ( 'NONE', #11689, 2.499999999999998668 ) ;
#23028 = PLANE ( 'NONE',  #22600 ) ;
#23029 = CONICAL_SURFACE ( 'NONE', #5962, 2.254620000000000513, 0.7853981633974461696 ) ;
#23030 = CARTESIAN_POINT ( 'NONE',  ( 35.24824457160689661, 8.315249525024576371, -27.55602540378494325 ) ) ;
#23031 = CALENDAR_DATE ( 2026, 31, 10 ) ;
#23032 = EDGE_CURVE ( 'NONE', #19524, #4472, #4025, .T. ) ;
#23033 = VERTEX_POINT ( 'NONE', #4493 ) ;
#23034 = DIRECTION ( 'NONE',  ( 0.000000000000000000, 0.000000000000000000, -1.000000000000000000 ) ) ;
#23035 = DIRECTION ( 'NONE',  ( -1.000000000000000000, 0.000000000000000000, 0.000000000000000000 ) ) ;
#23036 = ORIENTED_EDGE ( 'NONE', *, *, #17255, .T. ) ;
#23037 = AXIS2_PLACEMENT_3D ( 'NONE', #11515, #18754, #8040 ) ;
#23038 = EDGE_CURVE ( 'NONE', #17998, #10115, #13483, .T. ) ;
#23039 = DIRECTION ( 'NONE',  ( -0.9730401042858024541, 0.2306359803922080898, 5.959266323863413074E-17 ) ) ;
#23041 = AXIS2_PLACEMENT_3D ( 'NONE', #18225, #1946, #19656 ) ;
#23040 = DIRECTION ( 'NONE',  ( -0.5249589903860224505, 0.8511275218278915311, 1.187479569643817911E-16 ) ) ;
#23042 = FACE_OUTER_BOUND ( 'NONE', #18543, .T. ) ;
#23043 = EDGE_LOOP ( 'NONE', ( #14250, #10109, #1129, #17694, #14931 ) ) ;
#23044 = CARTESIAN_POINT ( 'NONE',  ( 2.500000000000000000, -17.30000000000000071, -2.500000000000000000 ) ) ;
#23045 = ADVANCED_FACE ( 'NONE', ( #20414 ), #22414, .T. ) ;
#23046 = SHAPE_DEFINITION_REPRESENTATION ( #13633, #22961 ) ;
#23048 = ADVANCED_FACE ( 'NONE', ( #9371 ), #13413, .F. ) ;
#23047 = ORIENTED_EDGE ( 'NONE', *, *, #21001, .T. ) ;
#23049 = ORIENTED_EDGE ( 'NONE', *, *, #2394, .T. ) ;
#23050 = CARTESIAN_POINT ( 'NONE',  ( -20.00000000397459843, 22.95208919257349933, -7.999999999995569766 ) ) ;
#23051 = CARTESIAN_POINT ( 'NONE',  ( -27.00000000000000000, -27.34999999999999787, -6.250000000000000000 ) ) ;
#23052 = DIRECTION ( 'NONE',  ( 7.946519521424616013E-35, 4.132425482310360071E-19, 1.000000000000000000 ) ) ;
#23053 = CALENDAR_DATE ( 2026, 31, 10 ) ;
#23054 = CARTESIAN_POINT ( 'NONE',  ( 35.66958329621319734, 8.215381216001370390, -29.25000000000050093 ) ) ;
#23055 = DIRECTION ( 'NONE',  ( -2.269747459788990007E-13, -2.220446049250330436E-15, -1.000000000000000000 ) ) ;
#23056 = AXIS2_PLACEMENT_3D ( 'NONE', #2332, #8036, #4230 ) ;
#23057 = CARTESIAN_POINT ( 'NONE',  ( -26.75617730459320143, 6.359992804688110901, 2.500999999999740098 ) ) ;
#23058 = AXIS2_PLACEMENT_3D ( 'NONE', #15593, #17495, #15361 ) ;
#23059 = DATE_AND_TIME ( #18493, #6456 ) ;
#23060 = VERTEX_POINT ( 'NONE', #16596 ) ;
#23061 = FACE_OUTER_BOUND ( 'NONE', #5692, .T. ) ;
#23062 = DATE_AND_TIME ( #11952, #3840 ) ;
#23063 = CARTESIAN_POINT ( 'NONE',  ( 37.20029037402979100, 11.08292547562999353, 8.849039310734006847 ) ) ;
#23064 = DIRECTION ( 'NONE',  ( -0.9730401042858035643, 0.2306359803922028717, 5.959266323858677443E-17 ) ) ;
#23065 = DIRECTION ( 'NONE',  ( -1.578894428126670167E-37, -2.578073951805180219E-21, 1.000000000000000000 ) ) ;
#23066 = CARTESIAN_POINT ( 'NONE',  ( 0.000000000000000000, 0.000000000000000000, -2.500000000000000000 ) ) ;
#23067 = CARTESIAN_POINT ( 'NONE',  ( 117.0319250210129951, -13.02226701625849969, -15.90000000000000036 ) ) ;
#23068 = VERTEX_POINT ( 'NONE', #321 ) ;
#23069 = DIRECTION ( 'NONE',  ( -0.07397971354964408275, -0.9972597464969258363, 2.255140518769849223E-15 ) ) ;
#23070 = ORIENTED_EDGE ( 'NONE', *, *, #2845, .T. ) ;
#23071 = DIRECTION ( 'NONE',  ( -1.466984912809909902E-16, -2.805478249466345005E-20, -1.000000000000000000 ) ) ;
#23072 = AXIS2_PLACEMENT_3D ( 'NONE', #6673, #13448, #19689 ) ;
#23073 = CARTESIAN_POINT ( 'NONE',  ( -26.68881687192900287, -6.639832696913689603, 2.500292893218909906 ) ) ;
#23074 = ORIENTED_EDGE ( 'NONE', *, *, #8368, .T. ) ;
#23075 = CYLINDRICAL_SURFACE ( 'NONE', #8460, 8.250000000000001776 ) ;
#23076 = ORIENTED_EDGE ( 'NONE', *, *, #3873, .F. ) ;
#23077 = DIRECTION ( 'NONE',  ( 0.9999862922474492821, 0.005235963827108391054, 0.000000000000000000 ) ) ;
#23078 = PERSON_AND_ORGANIZATION_ROLE ( 'design_supplier' ) ;
#23079 = DIRECTION ( 'NONE',  ( 0.2306359803922028995, 0.9730401042858035643, -4.741332172907957521E-18 ) ) ;
#23080 = EDGE_CURVE ( 'NONE', #3586, #8816, #13857, .T. ) ;
#23081 = APPROVAL_STATUS ( 'not_yet_approved' ) ;
#23082 = DIRECTION ( 'NONE',  ( -0.9730401042858036753, 0.2306359803922028995, -2.740969466505749537E-16 ) ) ;
#23083 = CYLINDRICAL_SURFACE ( 'NONE', #15486, 3.750000000000000000 ) ;
#23084 = DIRECTION ( 'NONE',  ( 1.000000000000000000, 0.000000000000000000, 0.000000000000000000 ) ) ;
#23085 = FACE_BOUND ( 'NONE', #1435, .T. ) ;
#23086 = VERTEX_POINT ( 'NONE', #9628 ) ;
#23087 = DIRECTION ( 'NONE',  ( 1.304396158928240120E-15, 5.761557392269829876E-15, -1.000000000000000000 ) ) ;
#23088 = DIRECTION ( 'NONE',  ( -0.9730401042858024541, 0.2306359803922080898, 5.959266323858852472E-17 ) ) ;
#23089 = ORIENTED_EDGE ( 'NONE', *, *, #17108, .F. ) ;
#23090 =( BOUNDED_CURVE ( )  B_SPLINE_CURVE ( 2, ( #14650, #5619, #20237 ),
 .UNSPECIFIED., .F., .F. ) 
 B_SPLINE_CURVE_WITH_KNOTS ( ( 3, 3 ),
 ( 0.000000000000000000, 0.2928548593876180162 ),
 .UNSPECIFIED. ) 
 CURVE ( )  GEOMETRIC_REPRESENTATION_ITEM ( )  RATIONAL_B_SPLINE_CURVE ( ( 1.000000000000000000, 1.037954849302039850, 1.000000000000000000 ) ) 
 REPRESENTATION_ITEM ( '' )  );
#23091 = CC_DESIGN_APPROVAL ( #10254, ( #9089 ) ) ;
#23092 = DIRECTION ( 'NONE',  ( -2.982858504577314686E-17, 2.441916418604790135E-15, 1.000000000000000000 ) ) ;
#23093 = DIRECTION ( 'NONE',  ( 1.466984912809907930E-16, 2.805478249466195144E-20, 1.000000000000000000 ) ) ;
#23094 = ORIENTED_EDGE ( 'NONE', *, *, #14190, .F. ) ;
#23095 = CONTEXT_DEPENDENT_SHAPE_REPRESENTATION ( #23187, #21987 ) ;
#23096 = CARTESIAN_POINT ( 'NONE',  ( 59.43368109719860826, 4.124228161845699958, 3.772686752615189359E-14 ) ) ;
#23097 = VERTEX_POINT ( 'NONE', #7710 ) ;
#23098 = EDGE_LOOP ( 'NONE', ( #22436, #5859, #2172, #17721, #13881, #7761, #17602, #12275, #7033, #18257, #1507, #1518, #191, #10697 ) ) ;
#23099 = PERSON_AND_ORGANIZATION ( #11966, #8758 ) ;
#23100 = LINE ( 'NONE', #13981, #11864 ) ;
#23101 = EDGE_LOOP ( 'NONE', ( #10609, #16603, #9393, #5480 ) ) ;
#23102 = DIRECTION ( 'NONE',  ( 1.000000000000000000, -2.270069654138870255E-15, 7.403850011488566665E-46 ) ) ;
#23103 = DATE_AND_TIME ( #3184, #5782 ) ;
#23104 = ADVANCED_FACE ( 'NONE', ( #11298 ), #16848, .T. ) ;
#23105 = PRODUCT_DEFINITION_SHAPE ( 'NONE', 'NONE',  #6637 ) ;
#23106 = CARTESIAN_POINT ( 'NONE',  ( -17.47493720815329965, 28.95208920939580111, -5.499999999996149747 ) ) ;
#23107 =( GEOMETRIC_REPRESENTATION_CONTEXT ( 3 ) GLOBAL_UNCERTAINTY_ASSIGNED_CONTEXT ( ( #12522 ) ) GLOBAL_UNIT_ASSIGNED_CONTEXT ( ( #18441, #18677, #3806 ) ) REPRESENTATION_CONTEXT ( 'NONE', 'WORKASPACE' ) );
#23108 = AXIS2_PLACEMENT_3D ( 'NONE', #12834, #14498, #17833 ) ;
#23109 = APPROVAL ( #10316, 'UNKNOWN' ) ;
#23110 = CIRCLE ( 'NONE', #4845, 4.250000000000000000 ) ;
#23111 = DIRECTION ( 'NONE',  ( -0.9999862922474492821, -0.005235963827121951387, 1.239088197126291310E-16 ) ) ;
#23112 = ORIENTED_EDGE ( 'NONE', *, *, #13204, .T. ) ;
#23113 = EDGE_CURVE ( 'NONE', #18898, #20737, #2483, .T. ) ;
#23114 = EDGE_CURVE ( 'NONE', #19111, #6605, #21807, .T. ) ;
#23115 = ORIENTED_EDGE ( 'NONE', *, *, #21471, .F. ) ;
#23116 = DIRECTION ( 'NONE',  ( -0.9730401042858024541, 0.2306359803922080898, 5.959266323858942451E-17 ) ) ;
#23117 = CARTESIAN_POINT ( 'NONE',  ( 28.07896398525720016, -3.287439373930470143, -14.50000000000040146 ) ) ;
#23118 = EDGE_LOOP ( 'NONE', ( #22196, #10556, #10730, #15841 ) ) ;
#23119 = APPROVAL_PERSON_ORGANIZATION ( #16380, #17811, #13072 ) ;
#23120 = CARTESIAN_POINT ( 'NONE',  ( 37.01481097301078194, 22.79827665208033594, 11.00000000000000178 ) ) ;
#23121 = VERTEX_POINT ( 'NONE', #6393 ) ;
#23122 = AXIS2_PLACEMENT_3D ( 'NONE', #14551, #21895, #5518 ) ;
#23123 = EDGE_LOOP ( 'NONE', ( #1454, #16557, #3173, #22040 ) ) ;
#23124 = DIRECTION ( 'NONE',  ( 0.8648054144888007722, 0.5021071549687909918, 5.295409231245618283E-17 ) ) ;
#23125 = VERTEX_POINT ( 'NONE', #17213 ) ;
#23126 = APPROVAL_ROLE ( '' ) ;
#23127 = VERTEX_POINT ( 'NONE', #8179 ) ;
#23128 = ORIENTED_EDGE ( 'NONE', *, *, #16504, .T. ) ;
#23129 = DIRECTION ( 'NONE',  ( -0.9730401042858035643, 0.2306359803922028717, -2.804983810440358308E-16 ) ) ;
#23130 = DATE_AND_TIME ( #8440, #3858 ) ;
#23131 = CIRCLE ( 'NONE', #19728, 1.000000000000000000 ) ;
#23132 = EDGE_CURVE ( 'NONE', #15046, #6087, #14614, .T. ) ;
#23133 = DIRECTION ( 'NONE',  ( -0.2306359803922032603, -0.9730401042858035643, 4.741332172907965995E-18 ) ) ;
#23134 = CIRCLE ( 'NONE', #12911, 0.0009999999999996990463 ) ;
#23135 = APPROVAL ( #18251, 'UNSPECIFIED' ) ;
#23136 = CC_DESIGN_APPROVAL ( #5465, ( #22291 ) ) ;
#23137 = CC_DESIGN_PERSON_AND_ORGANIZATION_ASSIGNMENT ( #5863, #21797, ( #19398 ) ) ;
#23138 = CC_DESIGN_APPROVAL ( #5101, ( #1155 ) ) ;
#23139 = CARTESIAN_POINT ( 'NONE',  ( -20.00000000000190070, -20.00000000000000000, -8.249999999995459632 ) ) ;
#23140 = EDGE_CURVE ( 'NONE', #9426, #12125, #15654, .T. ) ;
#23141 = ADVANCED_FACE ( 'NONE', ( #6870 ), #15881, .F. ) ;
#23142 = PERSON_AND_ORGANIZATION ( #11966, #8758 ) ;
#23143 = ADVANCED_FACE ( 'NONE', ( #2834 ), #15407, .F. ) ;
#23144 = ORIENTED_EDGE ( 'NONE', *, *, #7453, .T. ) ;
#23145 = PLANE ( 'NONE',  #21258 ) ;
#23146 = CARTESIAN_POINT ( 'NONE',  ( 35.35837847849400362, 22.00420084508149898, -15.00000000000049916 ) ) ;
#23147 = VECTOR ( 'NONE', #22567, 1000.000000000000000 ) ;
#23148 = ORIENTED_EDGE ( 'NONE', *, *, #5443, .F. ) ;
#23149 = CARTESIAN_POINT ( 'NONE',  ( 117.1933702072879981, -12.34113894325849969, -18.89999999999999858 ) ) ;
#23150 = CARTESIAN_POINT ( 'NONE',  ( -20.00000001748614054, -17.37500000000000000, 8.250000000004545697 ) ) ;
#23151 = DIRECTION ( 'NONE',  ( -6.123230199561459225E-17, -4.868008300101910084E-15, -1.000000000000000000 ) ) ;
#23152 = VERTEX_POINT ( 'NONE', #11997 ) ;
#23153 = CARTESIAN_POINT ( 'NONE',  ( -19.99975861755289941, 22.95209442650110176, 3.749999999999949818 ) ) ;
#23154 = CLOSED_SHELL ( 'NONE', ( #840, #21530, #2165, #9844, #15439, #11950, #324, #8402, #925, #14784, #5898, #15466, #6428, #15307, #9117, #22575, #22430, #340, #6822, #1538, #15417 ) ) ;
#23155 = PERSON_AND_ORGANIZATION ( #11966, #8758 ) ;
#23156 = PRODUCT_DEFINITION_FORMATION_WITH_SPECIFIED_SOURCE ( 'ANY', '', #1883, .NOT_KNOWN. ) ;
#23157 = ORIENTED_EDGE ( 'NONE', *, *, #22989, .F. ) ;
#23158 = ORIENTED_EDGE ( 'NONE', *, *, #1139, .F. ) ;
#23159 = FACE_OUTER_BOUND ( 'NONE', #10228, .T. ) ;
#23160 = CARTESIAN_POINT ( 'NONE',  ( 26.57755037370660034, -6.586732293729940402, 18.00000000000000000 ) ) ;
#23161 = LOCAL_TIME ( 14, 11, 27.00000000000000000, #5712 ) ;
#23162 = LINE ( 'NONE', #1439, #4618 ) ;
#23163 = SECURITY_CLASSIFICATION_LEVEL ( 'unclassified' ) ;
#23164 = CARTESIAN_POINT ( 'NONE',  ( 30.97225804683763073, 10.87033058831624466, -26.88000000000050349 ) ) ;
#23165 = AXIS2_PLACEMENT_3D ( 'NONE', #9607, #2692, #7926 ) ;
#23166 = EDGE_CURVE ( 'NONE', #13977, #2098, #4730, .T. ) ;
#23167 = DIRECTION ( 'NONE',  ( 0.1997366180463769070, 0.8426774492125652660, 0.5000000000000003331 ) ) ;
#23168 = LOCAL_TIME ( 14, 11, 27.00000000000000000, #6754 ) ;
#23169 = CIRCLE ( 'NONE', #15153, 2.500000000000000000 ) ;
#23170 = ADVANCED_FACE ( 'NONE', ( #2944, #8416, #4611 ), #10093, .T. ) ;
#23171 = EDGE_CURVE ( 'NONE', #11204, #12615, #9704, .T. ) ;
#23172 = VERTEX_POINT ( 'NONE', #20873 ) ;
#23173 = CARTESIAN_POINT ( 'NONE',  ( 58.25686728443110951, 17.76335315678753801, 10.49999999999999822 ) ) ;
#23174 = CALENDAR_DATE ( 2026, 31, 10 ) ;
#23175 = CC_DESIGN_SECURITY_CLASSIFICATION ( #5355, ( #19768 ) ) ;
#23176 = LOCAL_TIME ( 14, 11, 27.00000000000000000, #15911 ) ;
#23177 = CARTESIAN_POINT ( 'NONE',  ( 37.49471903941907414, 10.63079050866130970, 8.911849358505318008 ) ) ;
#23178 = AXIS2_PLACEMENT_3D ( 'NONE', #2489, #18652, #21945 ) ;
#23179 = FACE_OUTER_BOUND ( 'NONE', #16395, .T. ) ;
#23180 = CONICAL_SURFACE ( 'NONE', #1568, 1.033499999999999863, 1.029744258676650093 ) ;
#23181 = CARTESIAN_POINT ( 'NONE',  ( -22.50000000000000000, -20.00000000000000000, -2.500000000000000000 ) ) ;
#23182 = DIRECTION ( 'NONE',  ( 1.000000000000000000, 1.248400535696349791E-16, 5.473822126268819266E-49 ) ) ;
#23183 = CYLINDRICAL_SURFACE ( 'NONE', #9958, 2.500000000000000444 ) ;
#23184 = ORIENTED_EDGE ( 'NONE', *, *, #4749, .F. ) ;
#23185 = CC_DESIGN_APPROVAL ( #4416, ( #62 ) ) ;
#23186 = CARTESIAN_POINT ( 'NONE',  ( -16.00004797695773107, -0.08377682083104275035, -8.699586588110780178E-14 ) ) ;
#23187 =( REPRESENTATION_RELATIONSHIP ('NONE','NONE', #19303, #10375 ) REPRESENTATION_RELATIONSHIP_WITH_TRANSFORMATION ( #8401 )SHAPE_REPRESENTATION_RELATIONSHIP( ) );
#23188 = EDGE_LOOP ( 'NONE', ( #15578, #12140, #20107, #6145 ) ) ;
#23189 = LINE ( 'NONE', #19528, #12255 ) ;
#23190 = CARTESIAN_POINT ( 'NONE',  ( 53.10252809683450437, 27.27557781334509812, 3.299332471243299474E-14 ) ) ;
#23191 = VERTEX_POINT ( 'NONE', #1278 ) ;
#23192 = LINE ( 'NONE', #13950, #15658 ) ;
#23194 = ORIENTED_EDGE ( 'NONE', *, *, #10567, .T. ) ;
#23193 = EDGE_CURVE ( 'NONE', #18943, #18146, #13758, .T. ) ;
#23195 = CC_DESIGN_SECURITY_CLASSIFICATION ( #14859, ( #10349 ) ) ;
#23196 = DIRECTION ( 'NONE',  ( 0.000000000000000000, 0.000000000000000000, -1.000000000000000000 ) ) ;
#23197 = APPROVAL_ROLE ( '' ) ;
#23198 = AXIS2_PLACEMENT_3D ( 'NONE', #5039, #987, #8365 ) ;
#23199 = DIRECTION ( 'NONE',  ( 1.000000000000000000, 1.296622928517386003E-46, -1.245534812201467949E-169 ) ) ;
#23200 = VECTOR ( 'NONE', #15401, 1000.000000000000000 ) ;
#23201 = CIRCLE ( 'NONE', #19806, 2.500000000000000444 ) ;
#23202 = EDGE_CURVE ( 'NONE', #15872, #13648, #3613, .T. ) ;
#23203 =( LENGTH_UNIT ( ) NAMED_UNIT ( * ) SI_UNIT ( .MILLI., .METRE. ) );
#23204 = ORGANIZATION ( 'NAUO-ORG31', 'UNSPECIFIED', 'UNSPECIFIED' ) ;
#23205 = CARTESIAN_POINT ( 'NONE',  ( 27.73073027566760018, -1.721531772300955110, 13.00000000000000000 ) ) ;
#23206 = EDGE_CURVE ( 'NONE', #22534, #1609, #19217, .T. ) ;
#23207 = AXIS2_PLACEMENT_3D ( 'NONE', #18065, #16273, #4606 ) ;
#23208 = DIRECTION ( 'NONE',  ( 0.000000000000000000, 0.000000000000000000, -1.000000000000000000 ) ) ;
#23209 = CARTESIAN_POINT ( 'NONE',  ( 0.000000000000000000, 0.000000000000000000, 0.000000000000000000 ) ) ;
#23210 = VECTOR ( 'NONE', #592, 1000.000000000000114 ) ;
#23211 = CARTESIAN_POINT ( 'NONE',  ( 62.20574963825990267, 1.227340145578220021, -4.500000000000000000 ) ) ;
#23212 = ORIENTED_EDGE ( 'NONE', *, *, #558, .T. ) ;
#23213 = DIRECTION ( 'NONE',  ( -0.0007613694435018768464, 0.9999997101582432935, 0.000000000000000000 ) ) ;
#23214 = DESIGN_CONTEXT ( 'detailed design', #11583, 'design' ) ;
#23215 = LOCAL_TIME ( 14, 11, 27.00000000000000000, #5919 ) ;
#23216 = CARTESIAN_POINT ( 'NONE',  ( 102.2474456857739966, -6.023754975411469204, 3.510479034365399954E-14 ) ) ;
#23217 = VERTEX_POINT ( 'NONE', #21006 ) ;
#23218 = CARTESIAN_POINT ( 'NONE',  ( 5.000000000000000000, -27.34999999999999787, -5.000000000000000000 ) ) ;
#23219 = CIRCLE ( 'NONE', #5784, 3.499999999999998224 ) ;
#23220 = CARTESIAN_POINT ( 'NONE',  ( 35.24824457160688240, 8.315249525024842825, 27.55602540378454535 ) ) ;
#23221 = AXIS2_PLACEMENT_3D ( 'NONE', #1958, #22021, #14564 ) ;
#23222 = VERTEX_POINT ( 'NONE', #10210 ) ;
#23223 = COORDINATED_UNIVERSAL_TIME_OFFSET ( 0, 0, .AHEAD. ) ;
#23224 = AXIS2_PLACEMENT_3D ( 'NONE', #1962, #16452, #7440 ) ;
#23225 = CARTESIAN_POINT ( 'NONE',  ( -17.25000000397036715, 22.95208919256889857, 8.500000000003836931 ) ) ;
#23226 = ORIENTED_EDGE ( 'NONE', *, *, #14272, .T. ) ;
#23227 = ORIENTED_EDGE ( 'NONE', *, *, #14075, .F. ) ;
#23228 = APPLICATION_CONTEXT ( 'configuration controlled 3d designs of mechanical parts and assemblies' ) ;
#23229 = CALENDAR_DATE ( 2026, 31, 10 ) ;
#23230 = VECTOR ( 'NONE', #3010, 1000.000000000000114 ) ;
#23231 = DIRECTION ( 'NONE',  ( 0.9730401042858035643, -0.2306359803922028717, -5.959266323858677443E-17 ) ) ;
#23232 = ORIENTED_EDGE ( 'NONE', *, *, #6641, .F. ) ;
#23233 = CARTESIAN_POINT ( 'NONE',  ( -1.262685242559879909E-14, -17.30000000000000071, 5.000000000000000000 ) ) ;
#23234 = AXIS2_PLACEMENT_3D ( 'NONE', #2479, #7939, #22055 ) ;
#23235 = PERSON_AND_ORGANIZATION_ROLE ( 'design_owner' ) ;
#23236 = AXIS2_PLACEMENT_3D ( 'NONE', #10478, #12137, #15909 ) ;
#23237 = CC_DESIGN_PERSON_AND_ORGANIZATION_ASSIGNMENT ( #20328, #22212, ( #19756 ) ) ;
#23238 = APPROVAL_PERSON_ORGANIZATION ( #20268, #2413, #13252 ) ;
#23239 = CARTESIAN_POINT ( 'NONE',  ( -67.06978017061331343, -25.35162245663349978, -2.500000000000000000 ) ) ;
#23240 = AXIS2_PLACEMENT_3D ( 'NONE', #4279, #9505, #14837 ) ;
#23241 = PERSON ( 'NAUO-PER11', 'UNSPECIFIED', 'UNSPECIFIED', ('UNSPECIFIED'), ('UNSPECIFIED'), ('UNSPECIFIED') ) ;
#23242 = CIRCLE ( 'NONE', #14543, 0.1000000000000028644 ) ;
#23243 = SHAPE_REPRESENTATION ( 'Arm', ( #15545, #13649, #19715, #1887 ), #355 ) ;
#23244 = DIRECTION ( 'NONE',  ( 0.5249589903860194529, -0.8511275218278935295, 5.444325428271645316E-17 ) ) ;
#23245 = ORIENTED_EDGE ( 'NONE', *, *, #14892, .T. ) ;
#23246 = ORIENTED_EDGE ( 'NONE', *, *, #9353, .F. ) ;
#23247 = AXIS2_PLACEMENT_3D ( 'NONE', #19770, #10646, #18355 ) ;
#23248 = CARTESIAN_POINT ( 'NONE',  ( -17.00003426920497418, -0.08901278465814893570, 2.499999999999999556 ) ) ;
#23249 = DIRECTION ( 'NONE',  ( 0.7806762821593211665, -0.6249356306643909509, -7.632783294297951215E-15 ) ) ;
#23250 = VERTEX_POINT ( 'NONE', #17435 ) ;
#23251 = ADVANCED_FACE ( 'NONE', ( #21106 ), #15775, .F. ) ;
#23252 = APPROVAL_PERSON_ORGANIZATION ( #16649, #2233, #20242 ) ;
#23253 = DIRECTION ( 'NONE',  ( -6.123230199561429643E-17, -4.868008300101910084E-15, -1.000000000000000000 ) ) ;
#23254 = CARTESIAN_POINT ( 'NONE',  ( 39.37089837072289811, 22.23982225285509884, 13.00000000000000000 ) ) ;
#23255 = ORIENTED_EDGE ( 'NONE', *, *, #412, .F. ) ;
#23256 = CIRCLE ( 'NONE', #21753, 2.500000000000000888 ) ;
#23257 = ORIENTED_EDGE ( 'NONE', *, *, #1764, .F. ) ;
#23258 = DATE_AND_TIME ( #21932, #9138 ) ;
#23259 = ORIENTED_EDGE ( 'NONE', *, *, #6489, .T. ) ;
#23260 = VECTOR ( 'NONE', #17312, 1000.000000000000000 ) ;
#23261 = VERTEX_POINT ( 'NONE', #23106 ) ;
#23262 = CARTESIAN_POINT ( 'NONE',  ( 35.59419854219520118, 9.774809681453358934, -10.99076000000050080 ) ) ;
#23263 = CALENDAR_DATE ( 2026, 31, 10 ) ;
#23264 = EDGE_CURVE ( 'NONE', #22148, #16864, #10331, .T. ) ;
#23265 = DIRECTION ( 'NONE',  ( -0.2306359803922053142, -0.9730401042858028982, 0.000000000000000000 ) ) ;
#23266 = APPROVAL_ROLE ( '' ) ;
#23267 = CIRCLE ( 'NONE', #10401, 5.000000000000000888 ) ;
#23268 = AXIS2_PLACEMENT_3D ( 'NONE', #10305, #8391, #19659 ) ;
#23269 = CARTESIAN_POINT ( 'NONE',  ( 36.84099409957970295, 22.83947580187469839, -17.25000000000050093 ) ) ;
#23270 = CIRCLE ( 'NONE', #11944, 3.499999999999999556 ) ;
#23271 = CALENDAR_DATE ( 2026, 31, 10 ) ;
#23272 = VERTEX_POINT ( 'NONE', #8543 ) ;
#23273 = LINE ( 'NONE', #5789, #8377 ) ;
#23274 = DIRECTION ( 'NONE',  ( -0.2306359803922033436, -0.9730401042858034533, 0.000000000000000000 ) ) ;
#23275 = ORIENTED_EDGE ( 'NONE', *, *, #8804, .F. ) ;
#23276 = EDGE_CURVE ( 'NONE', #1644, #15703, #5092, .T. ) ;
#23277 = LINE ( 'NONE', #19603, #5599 ) ;
#23278 = FACE_OUTER_BOUND ( 'NONE', #3765, .T. ) ;
#23279 = CARTESIAN_POINT ( 'NONE',  ( -14.54830929662849925, 0.3367883020382200221, -5.499999999996749267 ) ) ;
#23280 = ORIENTED_EDGE ( 'NONE', *, *, #11385, .T. ) ;
#23281 = ORIENTED_EDGE ( 'NONE', *, *, #11578, .F. ) ;
#23282 = DIRECTION ( 'NONE',  ( -0.2306359803922031770, -0.9730401042858034533, 0.000000000000000000 ) ) ;
#23283 = APPROVAL ( #6610, 'UNSPECIFIED' ) ;
#23284 = COORDINATED_UNIVERSAL_TIME_OFFSET ( 0, 0, .AHEAD. ) ;
#23285 = AXIS2_PLACEMENT_3D ( 'NONE', #12667, #7542, #5631 ) ;
#23286 = ORIENTED_EDGE ( 'NONE', *, *, #18337, .T. ) ;
#23287 = CC_DESIGN_PERSON_AND_ORGANIZATION_ASSIGNMENT ( #22582, #10041, ( #6763 ) ) ;
#23288 = ORIENTED_EDGE ( 'NONE', *, *, #4480, .F. ) ;
#23289 = CARTESIAN_POINT ( 'NONE',  ( -20.00000000000000000, -20.00000000000000000, -5.000000000000000000 ) ) ;
#23290 = DIRECTION ( 'NONE',  ( -0.2306359803922032603, -0.9730401042858035643, 1.407521210652567579E-17 ) ) ;
#23291 = FACE_BOUND ( 'NONE', #19907, .T. ) ;
#23292 = CIRCLE ( 'NONE', #16094, 4.999999999999995559 ) ;
#23293 = PERSON_AND_ORGANIZATION_ROLE ( 'creator' ) ;
#23294 = EDGE_CURVE ( 'NONE', #11032, #3768, #18821, .T. ) ;
#23295 = DIRECTION ( 'NONE',  ( 5.798605125234323991E-17, -1.374421231021384554E-17, 1.000000000000000000 ) ) ;
#23296 = ADVANCED_FACE ( 'NONE', ( #16343 ), #1850, .F. ) ;
#23297 = PLANE ( 'NONE',  #11801 ) ;
#23298 = DIRECTION ( 'NONE',  ( 1.000000000000000000, 0.000000000000000000, 0.000000000000000000 ) ) ;
#23299 = CARTESIAN_POINT ( 'NONE',  ( -62.75934763415060047, -21.57895147295310068, -5.536226058455569256E-15 ) ) ;
#23300 = PERSON_AND_ORGANIZATION ( #11966, #8758 ) ;
#23301 = CARTESIAN_POINT ( 'NONE',  ( -20.00000000000000000, -20.00000000000000000, 2.500000000000000000 ) ) ;
#23302 = LINE ( 'NONE', #5607, #10145 ) ;
#23303 = EDGE_CURVE ( 'NONE', #21157, #8216, #6276, .T. ) ;
#23304 = DIRECTION ( 'NONE',  ( 4.063875459488295522E-16, -1.011971878839177951E-16, -1.000000000000000000 ) ) ;
#23305 = CARTESIAN_POINT ( 'NONE',  ( 36.78282996199610722, 11.03463321983559986, -29.25000000000050093 ) ) ;
#23306 = ORIENTED_EDGE ( 'NONE', *, *, #13196, .T. ) ;
#23307 = CARTESIAN_POINT ( 'NONE',  ( 114.8178196092480050, -22.36345201740219935, 13.00000000000000000 ) ) ;
#23308 = CC_DESIGN_PERSON_AND_ORGANIZATION_ASSIGNMENT ( #23025, #21243, ( #6911 ) ) ;
#23309 = PRODUCT ( '1602p_c_45', '1602p_c_45', '', ( #11216 ) ) ;
#23310 = CC_DESIGN_DATE_AND_TIME_ASSIGNMENT ( #8435, #19584, ( #14070 ) ) ;
#23311 = ORIENTED_EDGE ( 'NONE', *, *, #21762, .T. ) ;
#23312 = CARTESIAN_POINT ( 'NONE',  ( -22.99995202268987171, -0.1204285676208968203, -2.500000000000089706 ) ) ;
#23313 = DIRECTION ( 'NONE',  ( -0.9997648975362233292, -0.02168293463498000007, 0.000000000000000000 ) ) ;
#23314 = ORIENTED_EDGE ( 'NONE', *, *, #2161, .T. ) ;
#23315 = ADVANCED_FACE ( 'NONE', ( #19685 ), #179, .F. ) ;
#23316 = CARTESIAN_POINT ( 'NONE',  ( 31.14187293219668362, -1.979315439058051851, 11.00000000000020250 ) ) ;
#23317 = EDGE_CURVE ( 'NONE', #1465, #11510, #13115, .T. ) ;
#23318 = ORIENTED_EDGE ( 'NONE', *, *, #22177, .F. ) ;
#23319 = CIRCLE ( 'NONE', #4753, 2.500000000000000444 ) ;
#23320 = DIRECTION ( 'NONE',  ( -0.9730401042858036753, 0.2306359803922028995, 5.959266323858677443E-17 ) ) ;
#23321 = DATE_AND_TIME ( #16089, #3917 ) ;
#23322 = DIRECTION ( 'NONE',  ( 1.138590270679730064E-14, 2.220446049251240387E-15, 1.000000000000000000 ) ) ;
#23323 = DIRECTION ( 'NONE',  ( 2.306143273112860358E-15, 2.757014059715200372E-16, -1.000000000000000000 ) ) ;
#23324 = DIRECTION ( 'NONE',  ( 1.213490492418610097E-15, 4.861311874477940294E-15, 1.000000000000000000 ) ) ;
#23325 = DIRECTION ( 'NONE',  ( 0.000000000000000000, 0.000000000000000000, 1.000000000000000000 ) ) ;
#23326 = DIRECTION ( 'NONE',  ( -0.2306359803922080343, -0.9730401042858022320, 1.412237191019910313E-17 ) ) ;
#23327 = DIRECTION ( 'NONE',  ( 0.9822637906114334294, -0.1875042550281410536, 4.933538860811975815E-16 ) ) ;
#23328 = DIRECTION ( 'NONE',  ( -0.2306359803922026497, -0.9730401042858035643, 0.000000000000000000 ) ) ;
#23329 = ADVANCED_FACE ( 'NONE', ( #7341 ), #9234, .T. ) ;
#23330 = AXIS2_PLACEMENT_3D ( 'NONE', #18144, #20031, #18256 ) ;
#23331 = DIRECTION ( 'NONE',  ( -3.099353312215988811E-62, -9.818186930595456717E-93, 1.000000000000000000 ) ) ;
#23332 = EDGE_LOOP ( 'NONE', ( #20498, #22657 ) ) ;
#23333 = DIRECTION ( 'NONE',  ( 0.2306359803922080343, 0.9730401042858022320, -1.412237191019910313E-17 ) ) ;
#23334 = DIRECTION ( 'NONE',  ( -0.9997648976141148003, -0.02168293104353429673, 2.084710914536959359E-17 ) ) ;
#23335 = EDGE_LOOP ( 'NONE', ( #3672, #22367 ) ) ;
#23336 = CALENDAR_DATE ( 2026, 31, 10 ) ;
#23337 = CARTESIAN_POINT ( 'NONE',  ( 43.84419854219520829, 8.392275869980100359E-122, 21.49999999999999289 ) ) ;
#23338 = EDGE_LOOP ( 'NONE', ( #10929, #7129 ) ) ;
#23339 = ORIENTED_EDGE ( 'NONE', *, *, #6126, .F. ) ;
#23340 = ADVANCED_FACE ( 'NONE', ( #14225 ), #3644, .T. ) ;
#23341 = DATE_AND_TIME ( #12442, #13350 ) ;
#23342 = FACE_OUTER_BOUND ( 'NONE', #23188, .T. ) ;
#23343 = EDGE_LOOP ( 'NONE', ( #19586, #3538, #2558, #15613, #4966, #20022, #20724, #12573, #19602 ) ) ;
#23344 = EDGE_CURVE ( 'NONE', #14253, #14262, #15772, .T. ) ;
#23345 = CARTESIAN_POINT ( 'NONE',  ( 114.8178196092480050, -22.36345201740219935, 13.00000000000000000 ) ) ;
#23346 = DATE_AND_TIME ( #17787, #8081 ) ;
#23347 = DATE_TIME_ROLE ( 'classification_date' ) ;
#23348 = CARTESIAN_POINT ( 'NONE',  ( 52.45828777336780036, 19.13776831658130106, -13.00000000000000000 ) ) ;
#23349 = AXIS2_PLACEMENT_3D ( 'NONE', #18048, #3625, #7315 ) ;
#23350 = CARTESIAN_POINT ( 'NONE',  ( 33.90884364377009774, 10.17428291754599989, -28.47000000000049980 ) ) ;
#23351 = ORIENTED_EDGE ( 'NONE', *, *, #3286, .F. ) ;
#23352 = CARTESIAN_POINT ( 'NONE',  ( -20.00000000397420052, 22.95208919256889857, -6.499999999995379696 ) ) ;
#23353 = ORIENTED_EDGE ( 'NONE', *, *, #10309, .T. ) ;
#23354 = CARTESIAN_POINT ( 'NONE',  ( 121.1303491780936099, 5.207460461920159212, -13.00000000000000000 ) ) ;
#23355 = CARTESIAN_POINT ( 'NONE',  ( -22.50000000397270128, 22.95208917591822129, 5.500000000004487966 ) ) ;
#23356 = PLANE ( 'NONE',  #20356 ) ;
#23357 = ORIENTED_EDGE ( 'NONE', *, *, #13562, .T. ) ;
#23358 = CC_DESIGN_PERSON_AND_ORGANIZATION_ASSIGNMENT ( #23142, #1656, ( #7977 ) ) ;
#23359 = AXIS2_PLACEMENT_3D ( 'NONE', #7612, #13090, #20322 ) ;
#23360 = AXIS2_PLACEMENT_3D ( 'NONE', #19878, #3601, #10870 ) ;
#23361 = CARTESIAN_POINT ( 'NONE',  ( -62.73971250800079957, -25.32895006819559924, -5.538452170245418869E-15 ) ) ;
#23362 = LINE ( 'NONE', #1399, #19457 ) ;
#23363 = VERTEX_POINT ( 'NONE', #10566 ) ;
#23364 = VERTEX_POINT ( 'NONE', #12453 ) ;
#23365 = PERSON_AND_ORGANIZATION ( #11966, #8758 ) ;
#23366 = ORIENTED_EDGE ( 'NONE', *, *, #4262, .T. ) ;
#23367 = VERTEX_POINT ( 'NONE', #3752 ) ;
#23368 = DIRECTION ( 'NONE',  ( -0.2867834340965239592, 0.9579954394086668268, -6.596081495102488335E-32 ) ) ;
#23369 = PERSON_AND_ORGANIZATION ( #11966, #8758 ) ;
#23370 = CARTESIAN_POINT ( 'NONE',  ( -27.00000000000000000, -31.09999999999999787, 21.50000000000000000 ) ) ;
#23371 = COORDINATED_UNIVERSAL_TIME_OFFSET ( 0, 0, .AHEAD. ) ;
#23372 = ADVANCED_FACE ( 'NONE', ( #19797 ), #9109, .T. ) ;
#23373 = CIRCLE ( 'NONE', #2541, 2.066999999999999726 ) ;
#23374 = CIRCLE ( 'NONE', #18090, 2.066999999999997062 ) ;
#23375 = AXIS2_PLACEMENT_3D ( 'NONE', #14277, #7058, #5374 ) ;
#23376 =( NAMED_UNIT ( * ) SI_UNIT ( $, .STERADIAN. ) SOLID_ANGLE_UNIT ( ) );
#23377 = DIRECTION ( 'NONE',  ( 0.005235963827117092427, -0.9999862922474493931, -2.636227439667000721E-16 ) ) ;
#23378 = MECHANICAL_CONTEXT ( 'NONE', #21248, 'mechanical' ) ;
#23379 = ORIENTED_EDGE ( 'NONE', *, *, #2236, .T. ) ;
#23380 = CARTESIAN_POINT ( 'NONE',  ( -25.01253141238809974, 26.70208918381559826, -6.749999999994429345 ) ) ;
#23381 = DIRECTION ( 'NONE',  ( -0.2306359803922028440, -0.9730401042858034533, -4.307366329831518561E-32 ) ) ;
#23382 = VERTEX_POINT ( 'NONE', #17903 ) ;
#23383 = DIRECTION ( 'NONE',  ( -3.099353312215989243E-62, 2.689336210007789456E-77, 1.000000000000000000 ) ) ;
#23384 = CARTESIAN_POINT ( 'NONE',  ( -20.00000000000000000, -20.00000000000000000, 6.750000000004559908 ) ) ;
#23385 = DIRECTION ( 'NONE',  ( 0.000000000000000000, 0.000000000000000000, -1.000000000000000000 ) ) ;
#23386 = VECTOR ( 'NONE', #14398, 1000.000000000000000 ) ;
#23387 = VERTEX_POINT ( 'NONE', #1496 ) ;
#23388 = VERTEX_POINT ( 'NONE', #10802 ) ;
#23389 = DIRECTION ( 'NONE',  ( 0.8511275218278948618, 0.5249589903860170104, -5.212440122911309516E-17 ) ) ;
#23390 = ORIENTED_EDGE ( 'NONE', *, *, #20000, .F. ) ;
#23391 = DATE_AND_TIME ( #18308, #7248 ) ;
#23392 = AXIS2_PLACEMENT_3D ( 'NONE', #9196, #20113, #4198 ) ;
#23393 = EDGE_LOOP ( 'NONE', ( #15817, #18697, #11982, #13804, #15079, #20461, #7594, #3767, #1769, #15193, #1420, #787, #2478, #11068 ) ) ;
#23394 = ORIENTED_EDGE ( 'NONE', *, *, #15630, .T. ) ;
#23395 = DIRECTION ( 'NONE',  ( 0.9949874374308234071, 0.09999999677421649025, -2.262079412673754937E-13 ) ) ;
#23396 = DIRECTION ( 'NONE',  ( -0.005235963827108231460, 0.9999862922474493931, 2.671135040551741347E-18 ) ) ;
#23397 = VECTOR ( 'NONE', #15806, 1000.000000000000114 ) ;
#23398 = FACE_OUTER_BOUND ( 'NONE', #8146, .T. ) ;
#23399 = PERSON_AND_ORGANIZATION_ROLE ( 'creator' ) ;
#23400 = FACE_OUTER_BOUND ( 'NONE', #2910, .T. ) ;
#23401 = DIRECTION ( 'NONE',  ( -5.791496838535410422E-15, -2.469238035320170149E-14, 1.000000000000000000 ) ) ;
#23402 = VECTOR ( 'NONE', #4542, 999.9999999999998863 ) ;
#23403 =( REPRESENTATION_RELATIONSHIP ('NONE','NONE', #18771, #4456 ) REPRESENTATION_RELATIONSHIP_WITH_TRANSFORMATION ( #2176 )SHAPE_REPRESENTATION_RELATIONSHIP( ) );
#23404 = EDGE_CURVE ( 'NONE', #10146, #5108, #8692, .T. ) ;
#23405 = CARTESIAN_POINT ( 'NONE',  ( 0.000000000000000000, 0.000000000000000000, 0.000000000000000000 ) ) ;
#23406 = AXIS2_PLACEMENT_3D ( 'NONE', #6559, #21260, #6429 ) ;
#23407 = APPROVAL ( #19568, 'UNKNOWN' ) ;
#23409 = DIRECTION ( 'NONE',  ( -0.2306359803922031770, -0.9730401042858034533, 0.000000000000000000 ) ) ;
#23408 = AXIS2_PLACEMENT_3D ( 'NONE', #1475, #23087, #12094 ) ;
#23410 = COORDINATED_UNIVERSAL_TIME_OFFSET ( 0, 0, .AHEAD. ) ;
#23411 = AXIS2_PLACEMENT_3D ( 'NONE', #6335, #15473, #6444 ) ;
#23412 = CIRCLE ( 'NONE', #22678, 2.500000000000000000 ) ;
#23413 = CYLINDRICAL_SURFACE ( 'NONE', #4177, 2.499999999999998668 ) ;
#23414 = CARTESIAN_POINT ( 'NONE',  ( 117.1933702072879981, -12.34113894325849969, -18.89999999999999858 ) ) ;
#23415 = EDGE_CURVE ( 'NONE', #13431, #21440, #16513, .T. ) ;
#23416 = EDGE_CURVE ( 'NONE', #1637, #6349, #5194, .T. ) ;
#23417 = DIRECTION ( 'NONE',  ( 5.964507377817269296E-17, 4.861311874385510251E-15, 1.000000000000000000 ) ) ;
#23418 = DIRECTION ( 'NONE',  ( -0.9730401042858024541, 0.2306359803922080898, 5.959266323858952312E-17 ) ) ;
#23419 = DIRECTION ( 'NONE',  ( 8.911056267098788616E-18, 1.998401444326210262E-15, 1.000000000000000000 ) ) ;
#23420 = VERTEX_POINT ( 'NONE', #1621 ) ;
#23421 = CIRCLE ( 'NONE', #2951, 6.000000000000109246 ) ;
#23422 = CARTESIAN_POINT ( 'NONE',  ( 35.59419854219520118, 9.774809681453278998, -21.50000000000000000 ) ) ;
#23423 = UNCERTAINTY_MEASURE_WITH_UNIT (LENGTH_MEASURE( 1.000000000000000082E-05 ), #7374, 'distance_accuracy_value', 'NONE');
#23424 = ORIENTED_EDGE ( 'NONE', *, *, #10531, .T. ) ;
#23425 = CARTESIAN_POINT ( 'NONE',  ( 116.5619150869516290, -6.333538388044982703, 3.459551998232740566E-14 ) ) ;
#23426 = CARTESIAN_POINT ( 'NONE',  ( -27.00000000000000000, -31.09999999999999787, 6.250000000000000000 ) ) ;
#23427 = AXIS2_PLACEMENT_3D ( 'NONE', #20626, #20497, #9825 ) ;
#23428 = EDGE_LOOP ( 'NONE', ( #22050, #16251, #17539, #2732, #10596, #12341 ) ) ;
#23429 = DIRECTION ( 'NONE',  ( -0.9730401042858024541, 0.2306359803922080898, 5.959266323858942451E-17 ) ) ;
#23430 = EDGE_LOOP ( 'NONE', ( #17869, #21234 ) ) ;
#23431 = CIRCLE ( 'NONE', #5622, 2.750000000000002220 ) ;
#23432 = COORDINATED_UNIVERSAL_TIME_OFFSET ( 0, 0, .AHEAD. ) ;
#23433 = DIRECTION ( 'NONE',  ( -2.269747459788999852E-13, -2.220446049250470459E-15, -1.000000000000000000 ) ) ;
#23434 = EDGE_CURVE ( 'NONE', #16110, #12330, #15371, .T. ) ;
#23435 =( NAMED_UNIT ( * ) SI_UNIT ( $, .STERADIAN. ) SOLID_ANGLE_UNIT ( ) );
#23436 = DIRECTION ( 'NONE',  ( -3.099353312215989243E-62, -1.635250850668769823E-78, 1.000000000000000000 ) ) ;
#23437 = APPROVAL ( #15405, 'UNSPECIFIED' ) ;
#23438 = FACE_OUTER_BOUND ( 'NONE', #21365, .T. ) ;
#23439 = DIRECTION ( 'NONE',  ( 0.000000000000000000, 0.000000000000000000, 1.000000000000000000 ) ) ;
#23440 = CC_DESIGN_PERSON_AND_ORGANIZATION_ASSIGNMENT ( #13166, #20174, ( #7624 ) ) ;
#23441 = LINE ( 'NONE', #3507, #10797 ) ;
#23442 = CARTESIAN_POINT ( 'NONE',  ( 3.174494135099829695, 19.69896361837129817, -4.500000000000000000 ) ) ;
#23443 = EDGE_CURVE ( 'NONE', #4562, #21997, #9001, .T. ) ;
#23444 = EDGE_CURVE ( 'NONE', #16863, #20782, #17284, .T. ) ;
#23445 = CARTESIAN_POINT ( 'NONE',  ( 2.500000000000000000, -28.60000000000000142, -21.50000000000000000 ) ) ;
#23446 = CARTESIAN_POINT ( 'NONE',  ( -19.49999999982360066, -0.1021026942259700004, 2.500000000000000000 ) ) ;
#23447 = CC_DESIGN_DATE_AND_TIME_ASSIGNMENT ( #19500, #2986, ( #19552 ) ) ;
#23448 = VECTOR ( 'NONE', #10018, 999.9999999999998863 ) ;
#23449 = EDGE_LOOP ( 'NONE', ( #21453, #2342, #17430, #16770 ) ) ;
#23450 = DIRECTION ( 'NONE',  ( 1.000000000000000000, 0.000000000000000000, 0.000000000000000000 ) ) ;
#23451 = FACE_OUTER_BOUND ( 'NONE', #13537, .T. ) ;
#23452 = VERTEX_POINT ( 'NONE', #10918 ) ;
#23453 = APPROVAL_ROLE ( '' ) ;
#23454 = DIRECTION ( 'NONE',  ( 0.9730401042858035643, -0.2306359803922028717, 6.356122819266969852E-16 ) ) ;
#23455 = ORIENTED_EDGE ( 'NONE', *, *, #20071, .F. ) ;
#23456 = SHAPE_DEFINITION_REPRESENTATION ( #17433, #5493 ) ;
#23457 = DIRECTION ( 'NONE',  ( -2.270069654138870255E-15, -1.000000000000000000, -7.035747901516317327E-77 ) ) ;
#23458 = VERTEX_POINT ( 'NONE', #21805 ) ;
#23459 = FACE_OUTER_BOUND ( 'NONE', #835, .T. ) ;
#23460 = APPROVAL_STATUS ( 'not_yet_approved' ) ;
#23461 = ADVANCED_FACE ( 'NONE', ( #15142 ), #16682, .T. ) ;
#23462 = APPROVAL_ROLE ( '' ) ;
#23463 = DIRECTION ( 'NONE',  ( -1.187319687680494078E-16, -2.805478249478345354E-20, -1.000000000000000000 ) ) ;
#23464 = LINE ( 'NONE', #10803, #3937 ) ;
#23465 = CIRCLE ( 'NONE', #16685, 2.650000000000001688 ) ;
#23466 = VERTEX_POINT ( 'NONE', #9462 ) ;
#23467 = FACE_OUTER_BOUND ( 'NONE', #10036, .T. ) ;
#23468 = EDGE_CURVE ( 'NONE', #8857, #15552, #20701, .T. ) ;
#23469 = EDGE_CURVE ( 'NONE', #8698, #5737, #4763, .T. ) ;
#23470 = ORIENTED_EDGE ( 'NONE', *, *, #19122, .F. ) ;
#23471 = DIRECTION ( 'NONE',  ( 0.000000000000000000, 1.020425574104004122E-16, 1.000000000000000000 ) ) ;
#23472 = CARTESIAN_POINT ( 'NONE',  ( 113.8430260960419957, 8.210644904773758412, -2.066999999999969528 ) ) ;
#23473 = CARTESIAN_POINT ( 'NONE',  ( 38.77124482170317066, 19.70991798171200671, 13.00000000000000000 ) ) ;
#23474 = NEXT_ASSEMBLY_USAGE_OCCURRENCE ( 'NAUO1', ' ', ' ', #4231, #10854, $ ) ;
#23475 = NEXT_ASSEMBLY_USAGE_OCCURRENCE ( 'NAUO2', ' ', ' ', #4231, #4578, $ ) ;
#23476 = NEXT_ASSEMBLY_USAGE_OCCURRENCE ( 'NAUO3', ' ', ' ', #4231, #3293, $ ) ;
#23477 = NEXT_ASSEMBLY_USAGE_OCCURRENCE ( 'NAUO4', ' ', ' ', #4231, #3714, $ ) ;
#23478 = NEXT_ASSEMBLY_USAGE_OCCURRENCE ( 'NAUO5', ' ', ' ', #4231, #22291, $ ) ;
#23479 = NEXT_ASSEMBLY_USAGE_OCCURRENCE ( 'NAUO6', ' ', ' ', #4231, #19552, $ ) ;
#23480 = NEXT_ASSEMBLY_USAGE_OCCURRENCE ( 'NAUO7', ' ', ' ', #4231, #14615, $ ) ;
#23481 = NEXT_ASSEMBLY_USAGE_OCCURRENCE ( 'NAUO8', ' ', ' ', #4231, #9386, $ ) ;
#23482 = NEXT_ASSEMBLY_USAGE_OCCURRENCE ( 'NAUO9', ' ', ' ', #4231, #7139, $ ) ;
#23483 = NEXT_ASSEMBLY_USAGE_OCCURRENCE ( 'NAUO10', ' ', ' ', #7139, #1978, $ ) ;
#23484 = NEXT_ASSEMBLY_USAGE_OCCURRENCE ( 'NAUO11', ' ', ' ', #7139, #4882, $ ) ;
#23485 = NEXT_ASSEMBLY_USAGE_OCCURRENCE ( 'NAUO12', ' ', ' ', #7139, #1591, $ ) ;
#23486 = NEXT_ASSEMBLY_USAGE_OCCURRENCE ( 'NAUO13', ' ', ' ', #7139, #12504, $ ) ;
#23487 = NEXT_ASSEMBLY_USAGE_OCCURRENCE ( 'NAUO14', ' ', ' ', #7139, #3051, $ ) ;
#23488 = NEXT_ASSEMBLY_USAGE_OCCURRENCE ( 'NAUO15', ' ', ' ', #7139, #19756, $ ) ;
#23489 = NEXT_ASSEMBLY_USAGE_OCCURRENCE ( 'NAUO16', ' ', ' ', #7139, #20770, $ ) ;
#23490 = NEXT_ASSEMBLY_USAGE_OCCURRENCE ( 'NAUO17', ' ', ' ', #7139, #6840, $ ) ;
#23491 = NEXT_ASSEMBLY_USAGE_OCCURRENCE ( 'NAUO18', ' ', ' ', #7139, #12089, $ ) ;
#23492 = NEXT_ASSEMBLY_USAGE_OCCURRENCE ( 'NAUO19', ' ', ' ', #3714, #13884, $ ) ;
#23493 = NEXT_ASSEMBLY_USAGE_OCCURRENCE ( 'NAUO20', ' ', ' ', #3714, #13468, $ ) ;
#23494 = NEXT_ASSEMBLY_USAGE_OCCURRENCE ( 'NAUO21', ' ', ' ', #3714, #8957, $ ) ;
#23495 = NEXT_ASSEMBLY_USAGE_OCCURRENCE ( 'NAUO22', ' ', ' ', #4578, #10554, $ ) ;
#23496 = NEXT_ASSEMBLY_USAGE_OCCURRENCE ( 'NAUO23', ' ', ' ', #4578, #5893, $ ) ;
#23497 = NEXT_ASSEMBLY_USAGE_OCCURRENCE ( 'NAUO24', ' ', ' ', #4578, #17062, $ ) ;
#23498 = NEXT_ASSEMBLY_USAGE_OCCURRENCE ( 'NAUO25', ' ', ' ', #4578, #1530, $ ) ;
#23499 = NEXT_ASSEMBLY_USAGE_OCCURRENCE ( 'NAUO26', ' ', ' ', #4578, #18095, $ ) ;
#23500 = NEXT_ASSEMBLY_USAGE_OCCURRENCE ( 'NAUO27', ' ', ' ', #4578, #10711, $ ) ;
#23501 = NEXT_ASSEMBLY_USAGE_OCCURRENCE ( 'NAUO28', ' ', ' ', #4578, #5042, $ ) ;
#23502 = NEXT_ASSEMBLY_USAGE_OCCURRENCE ( 'NAUO29', ' ', ' ', #4578, #13165, $ ) ;
#23503 = NEXT_ASSEMBLY_USAGE_OCCURRENCE ( 'NAUO30', ' ', ' ', #4578, #15459, $ ) ;
#23504 = NEXT_ASSEMBLY_USAGE_OCCURRENCE ( 'NAUO31', ' ', ' ', #4578, #19382, $ ) ;
#23505 = NEXT_ASSEMBLY_USAGE_OCCURRENCE ( 'NAUO32', ' ', ' ', #4578, #16907, $ ) ;
#23506 = NEXT_ASSEMBLY_USAGE_OCCURRENCE ( 'NAUO33', ' ', ' ', #4578, #6763, $ ) ;
#23507 = NEXT_ASSEMBLY_USAGE_OCCURRENCE ( 'NAUO34', ' ', ' ', #4578, #13725, $ ) ;
#23508 = NEXT_ASSEMBLY_USAGE_OCCURRENCE ( 'NAUO35', ' ', ' ', #4578, #6637, $ ) ;
#23509 = NEXT_ASSEMBLY_USAGE_OCCURRENCE ( 'NAUO36', ' ', ' ', #4578, #16771, $ ) ;
#23510 = NEXT_ASSEMBLY_USAGE_OCCURRENCE ( 'NAUO37', ' ', ' ', #4578, #18531, $ ) ;
#23511 = NEXT_ASSEMBLY_USAGE_OCCURRENCE ( 'NAUO38', ' ', ' ', #4578, #19247, $ ) ;
#23512 = NEXT_ASSEMBLY_USAGE_OCCURRENCE ( 'NAUO39', ' ', ' ', #10854, #20819, $ ) ;
#23513 = NEXT_ASSEMBLY_USAGE_OCCURRENCE ( 'NAUO40', ' ', ' ', #10854, #9377, $ ) ;
#23514 = NEXT_ASSEMBLY_USAGE_OCCURRENCE ( 'NAUO41', ' ', ' ', #10854, #9078, $ ) ;
#23515 = COLOUR_RGB('Deep Blue', 0.09019608, 0.27058824, 0.51372549);
#23516 = FILL_AREA_STYLE_COLOUR('',#23515);
#23517 = FILL_AREA_STYLE('',(#23516));
#23518 = SURFACE_STYLE_FILL_AREA(#23517);
#23519 = SURFACE_SIDE_STYLE('',(#23518));
#23520 = SURFACE_STYLE_USAGE(.BOTH.,#23519);
#23521 = PRESENTATION_STYLE_ASSIGNMENT((#23520));
#23522 = COLOUR_RGB('Light Blue', 0.66274510, 0.83137255, 0.94901961);
#23523 = FILL_AREA_STYLE_COLOUR('',#23522);
#23524 = FILL_AREA_STYLE('',(#23523));
#23525 = SURFACE_STYLE_FILL_AREA(#23524);
#23526 = SURFACE_SIDE_STYLE('',(#23525));
#23527 = SURFACE_STYLE_USAGE(.BOTH.,#23526);
#23528 = PRESENTATION_STYLE_ASSIGNMENT((#23527));
#23529 = COLOUR_RGB('Sky Blue', 0.31764706, 0.68627451, 0.89019608);
#23530 = FILL_AREA_STYLE_COLOUR('',#23529);
#23531 = FILL_AREA_STYLE('',(#23530));
#23532 = SURFACE_STYLE_FILL_AREA(#23531);
#23533 = SURFACE_SIDE_STYLE('',(#23532));
#23534 = SURFACE_STYLE_USAGE(.BOTH.,#23533);
#23535 = PRESENTATION_STYLE_ASSIGNMENT((#23534));
#23536 = COLOUR_RGB('Slate Gray', 0.40784314, 0.44705882, 0.49803922);
#23537 = FILL_AREA_STYLE_COLOUR('',#23536);
#23538 = FILL_AREA_STYLE('',(#23537));
#23539 = SURFACE_STYLE_FILL_AREA(#23538);
#23540 = SURFACE_SIDE_STYLE('',(#23539));
#23541 = SURFACE_STYLE_USAGE(.BOTH.,#23540);
#23542 = PRESENTATION_STYLE_ASSIGNMENT((#23541));
#23543 = COLOUR_RGB('Light Gray', 0.72549020, 0.75294118, 0.79215686);
#23544 = FILL_AREA_STYLE_COLOUR('',#23543);
#23545 = FILL_AREA_STYLE('',(#23544));
#23546 = SURFACE_STYLE_FILL_AREA(#23545);
#23547 = SURFACE_SIDE_STYLE('',(#23546));
#23548 = SURFACE_STYLE_USAGE(.BOTH.,#23547);
#23549 = PRESENTATION_STYLE_ASSIGNMENT((#23548));
#23550 = COLOUR_RGB('Black', 0.08235294, 0.09019608, 0.10196078);
#23551 = FILL_AREA_STYLE_COLOUR('',#23550);
#23552 = FILL_AREA_STYLE('',(#23551));
#23553 = SURFACE_STYLE_FILL_AREA(#23552);
#23554 = SURFACE_SIDE_STYLE('',(#23553));
#23555 = SURFACE_STYLE_USAGE(.BOTH.,#23554);
#23556 = PRESENTATION_STYLE_ASSIGNMENT((#23555));
#23557 = STYLED_ITEM('',(#23521),#1705);
#23558 = MECHANICAL_DESIGN_GEOMETRIC_PRESENTATION_REPRESENTATION('',(#23557),#22737);
#23559 = STYLED_ITEM('',(#23542),#17019);
#23560 = MECHANICAL_DESIGN_GEOMETRIC_PRESENTATION_REPRESENTATION('',(#23559),#15936);
#23561 = STYLED_ITEM('',(#23528),#16939);
#23562 = MECHANICAL_DESIGN_GEOMETRIC_PRESENTATION_REPRESENTATION('',(#23561),#21233);
#23563 = STYLED_ITEM('',(#23549),#17389);
#23564 = MECHANICAL_DESIGN_GEOMETRIC_PRESENTATION_REPRESENTATION('',(#23563),#10500);
#23565 = STYLED_ITEM('',(#23535),#1933);
#23566 = MECHANICAL_DESIGN_GEOMETRIC_PRESENTATION_REPRESENTATION('',(#23565),#2264);
#23567 = STYLED_ITEM('',(#23556),#9741);
#23568 = MECHANICAL_DESIGN_GEOMETRIC_PRESENTATION_REPRESENTATION('',(#23567),#21969);
#23569 = STYLED_ITEM('',(#23556),#9134);
#23570 = MECHANICAL_DESIGN_GEOMETRIC_PRESENTATION_REPRESENTATION('',(#23569),#6306);
#23571 = STYLED_ITEM('',(#23521),#17139);
#23572 = MECHANICAL_DESIGN_GEOMETRIC_PRESENTATION_REPRESENTATION('',(#23571),#19550);
#23573 = STYLED_ITEM('',(#23521),#1233);
#23574 = MECHANICAL_DESIGN_GEOMETRIC_PRESENTATION_REPRESENTATION('',(#23573),#3270);
#23575 = STYLED_ITEM('',(#23549),#9367);
#23576 = MECHANICAL_DESIGN_GEOMETRIC_PRESENTATION_REPRESENTATION('',(#23575),#1734);
#23577 = STYLED_ITEM('',(#23556),#17099);
#23578 = MECHANICAL_DESIGN_GEOMETRIC_PRESENTATION_REPRESENTATION('',(#23577),#9323);
#23579 = STYLED_ITEM('',(#23528),#9215);
#23580 = MECHANICAL_DESIGN_GEOMETRIC_PRESENTATION_REPRESENTATION('',(#23579),#1146);
#23581 = STYLED_ITEM('',(#23549),#9094);
#23582 = MECHANICAL_DESIGN_GEOMETRIC_PRESENTATION_REPRESENTATION('',(#23581),#10268);
#23583 = STYLED_ITEM('',(#23556),#1581);
#23584 = MECHANICAL_DESIGN_GEOMETRIC_PRESENTATION_REPRESENTATION('',(#23583),#15784);
#23585 = STYLED_ITEM('',(#23542),#17344);
#23586 = MECHANICAL_DESIGN_GEOMETRIC_PRESENTATION_REPRESENTATION('',(#23585),#19347);
#23587 = STYLED_ITEM('',(#23549),#9662);
#23588 = MECHANICAL_DESIGN_GEOMETRIC_PRESENTATION_REPRESENTATION('',(#23587),#23107);
#23589 = STYLED_ITEM('',(#23556),#17588);
#23590 = MECHANICAL_DESIGN_GEOMETRIC_PRESENTATION_REPRESENTATION('',(#23589),#20713);
#23591 = STYLED_ITEM('',(#23528),#1279);
#23592 = MECHANICAL_DESIGN_GEOMETRIC_PRESENTATION_REPRESENTATION('',(#23591),#13514);
#23593 = STYLED_ITEM('',(#23535),#1311);
#23594 = MECHANICAL_DESIGN_GEOMETRIC_PRESENTATION_REPRESENTATION('',(#23593),#11790);
#23595 = STYLED_ITEM('',(#23542),#1349);
#23596 = MECHANICAL_DESIGN_GEOMETRIC_PRESENTATION_REPRESENTATION('',(#23595),#21837);
#23597 = STYLED_ITEM('',(#23549),#17052);
#23598 = MECHANICAL_DESIGN_GEOMETRIC_PRESENTATION_REPRESENTATION('',(#23597),#1341);
#23599 = STYLED_ITEM('',(#23528),#1851);
#23600 = MECHANICAL_DESIGN_GEOMETRIC_PRESENTATION_REPRESENTATION('',(#23599),#7801);
#23601 = STYLED_ITEM('',(#23556),#9448);
#23602 = MECHANICAL_DESIGN_GEOMETRIC_PRESENTATION_REPRESENTATION('',(#23601),#3642);
#23603 = STYLED_ITEM('',(#23521),#9171);
#23604 = MECHANICAL_DESIGN_GEOMETRIC_PRESENTATION_REPRESENTATION('',(#23603),#21598);
#23605 = STYLED_ITEM('',(#23542),#9625);
#23606 = MECHANICAL_DESIGN_GEOMETRIC_PRESENTATION_REPRESENTATION('',(#23605),#22192);
#23607 = STYLED_ITEM('',(#23535),#17306);
#23608 = MECHANICAL_DESIGN_GEOMETRIC_PRESENTATION_REPRESENTATION('',(#23607),#4017);
#23609 = STYLED_ITEM('',(#23521),#17699);
#23610 = MECHANICAL_DESIGN_GEOMETRIC_PRESENTATION_REPRESENTATION('',(#23609),#20868);
#23611 = STYLED_ITEM('',(#23521),#9848);
#23612 = MECHANICAL_DESIGN_GEOMETRIC_PRESENTATION_REPRESENTATION('',(#23611),#5684);
#23613 = STYLED_ITEM('',(#23535),#16982);
#23614 = MECHANICAL_DESIGN_GEOMETRIC_PRESENTATION_REPRESENTATION('',(#23613),#14249);
#23615 = STYLED_ITEM('',(#23521),#9489);
#23616 = MECHANICAL_DESIGN_GEOMETRIC_PRESENTATION_REPRESENTATION('',(#23615),#743);
#23617 = STYLED_ITEM('',(#23535),#9291);
#23618 = MECHANICAL_DESIGN_GEOMETRIC_PRESENTATION_REPRESENTATION('',(#23617),#210);
#23619 = STYLED_ITEM('',(#23542),#2022);
#23620 = MECHANICAL_DESIGN_GEOMETRIC_PRESENTATION_REPRESENTATION('',(#23619),#14020);
#23621 = STYLED_ITEM('',(#23549),#1464);
#23622 = MECHANICAL_DESIGN_GEOMETRIC_PRESENTATION_REPRESENTATION('',(#23621),#15185);
#23623 = STYLED_ITEM('',(#23528),#17187);
#23624 = MECHANICAL_DESIGN_GEOMETRIC_PRESENTATION_REPRESENTATION('',(#23623),#11247);
#23625 = STYLED_ITEM('',(#23528),#9531);
#23626 = MECHANICAL_DESIGN_GEOMETRIC_PRESENTATION_REPRESENTATION('',(#23625),#2093);
#23627 = STYLED_ITEM('',(#23542),#9329);
#23628 = MECHANICAL_DESIGN_GEOMETRIC_PRESENTATION_REPRESENTATION('',(#23627),#16529);
#23629 = STYLED_ITEM('',(#23535),#9573);
#23630 = MECHANICAL_DESIGN_GEOMETRIC_PRESENTATION_REPRESENTATION('',(#23629),#3033);
ENDSEC;
END-ISO-10303-21;
